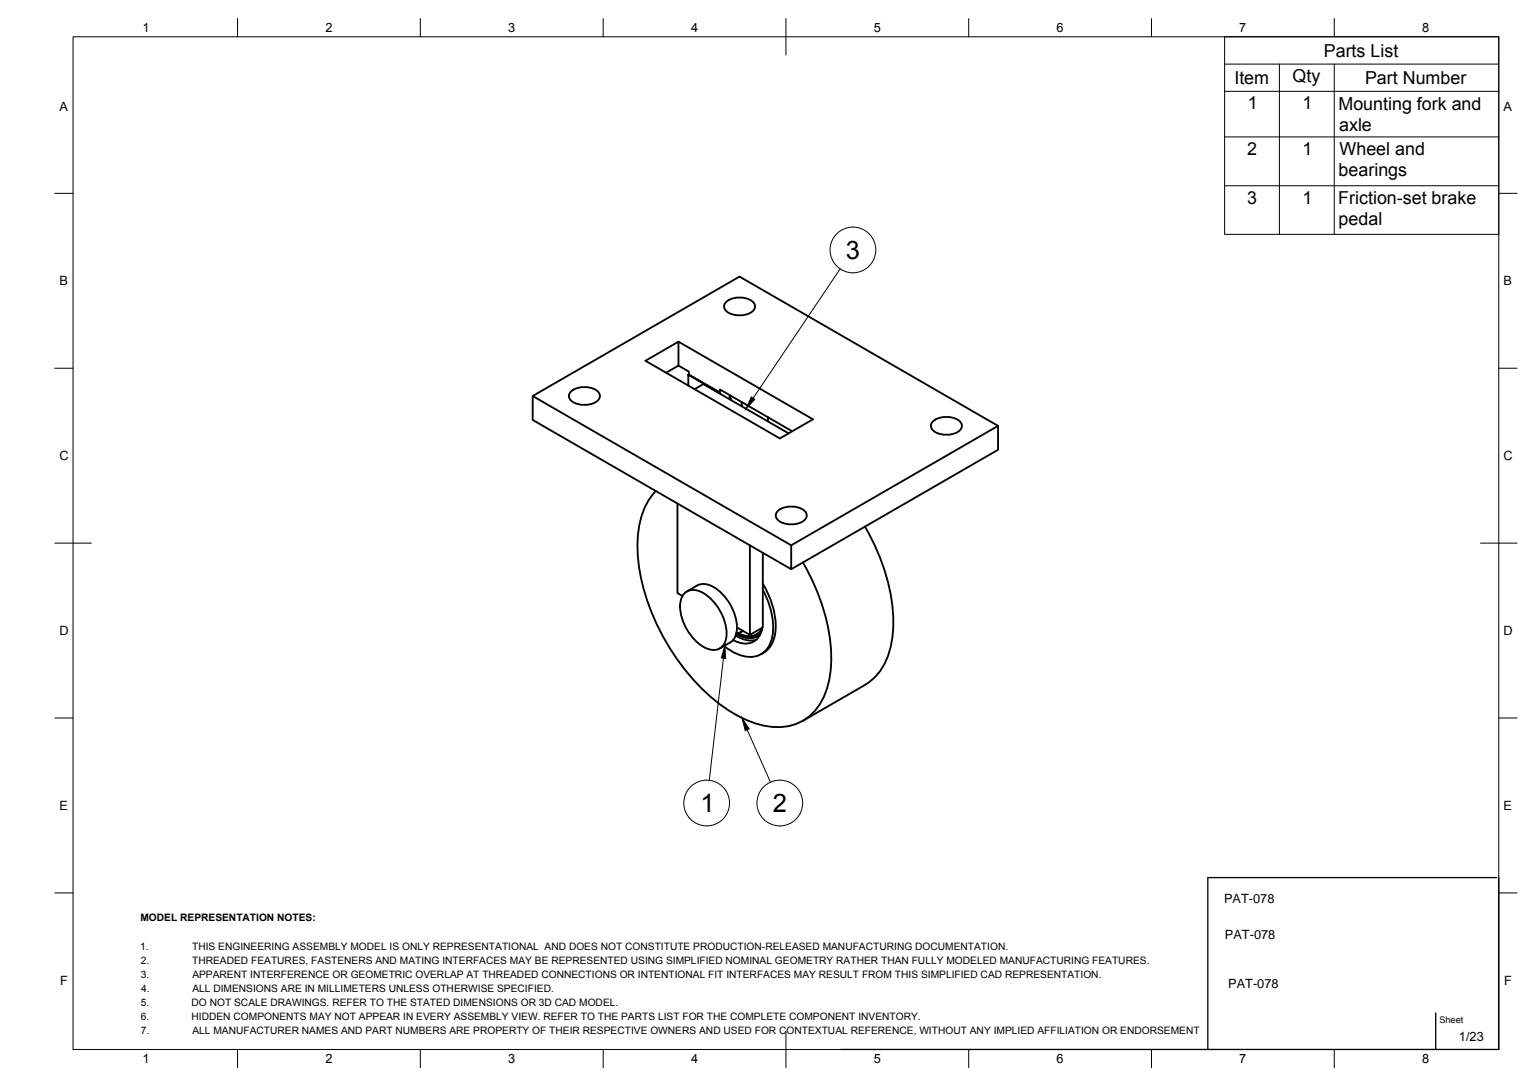
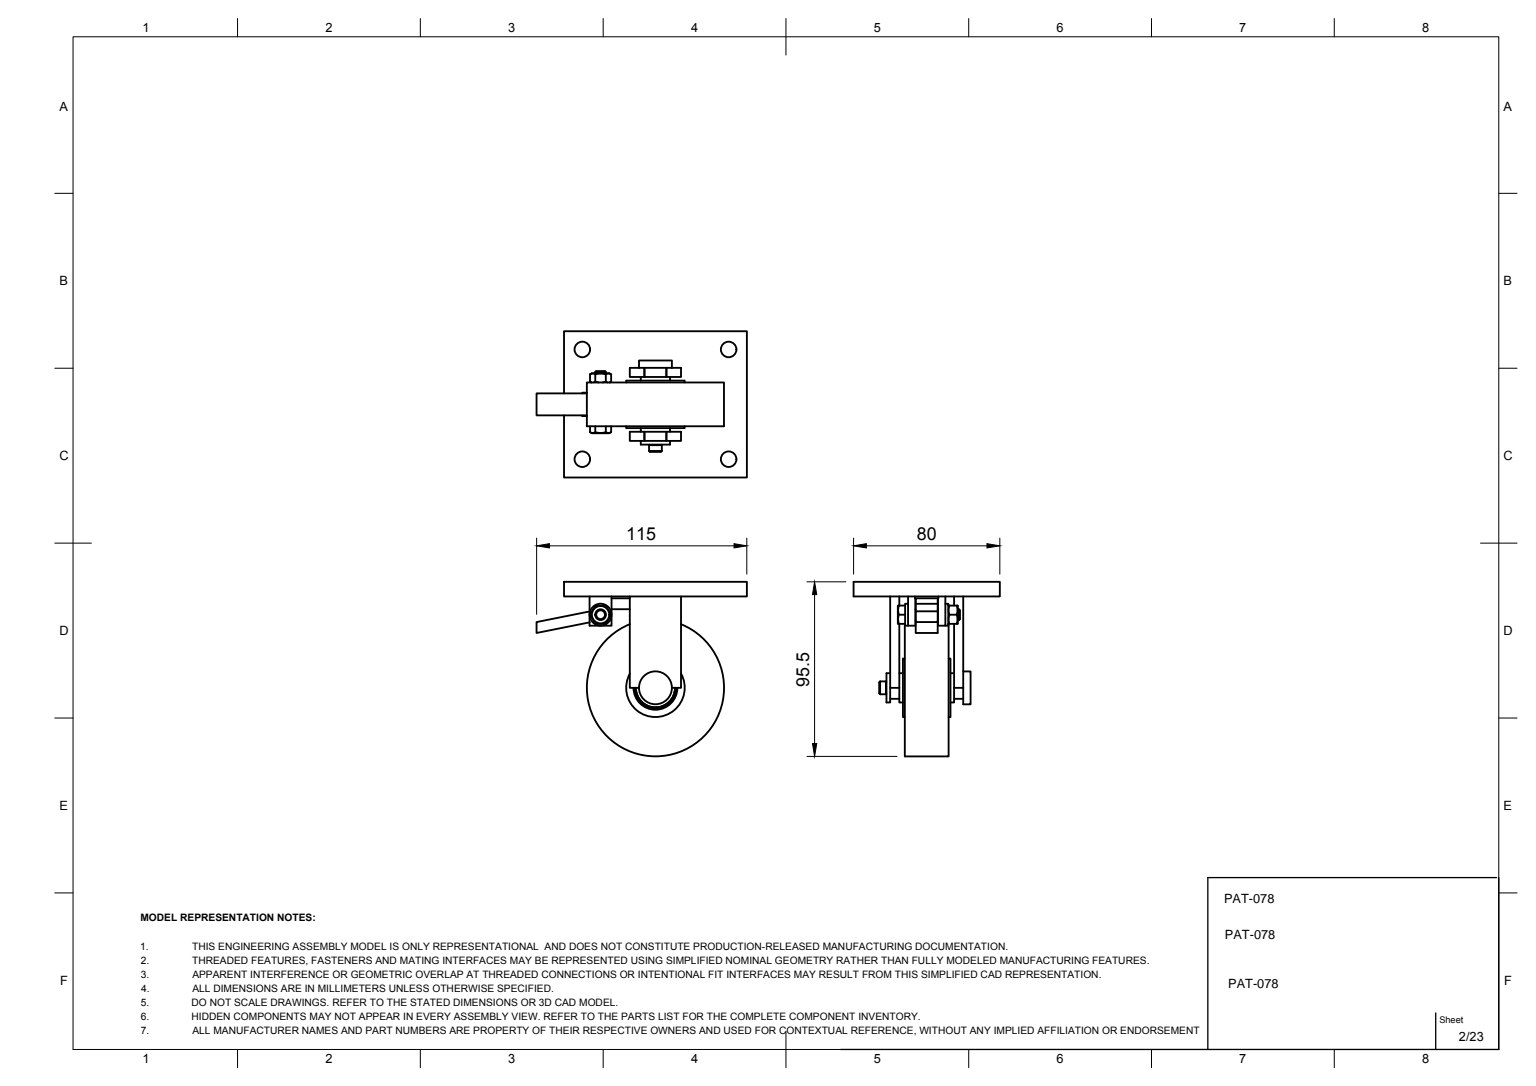
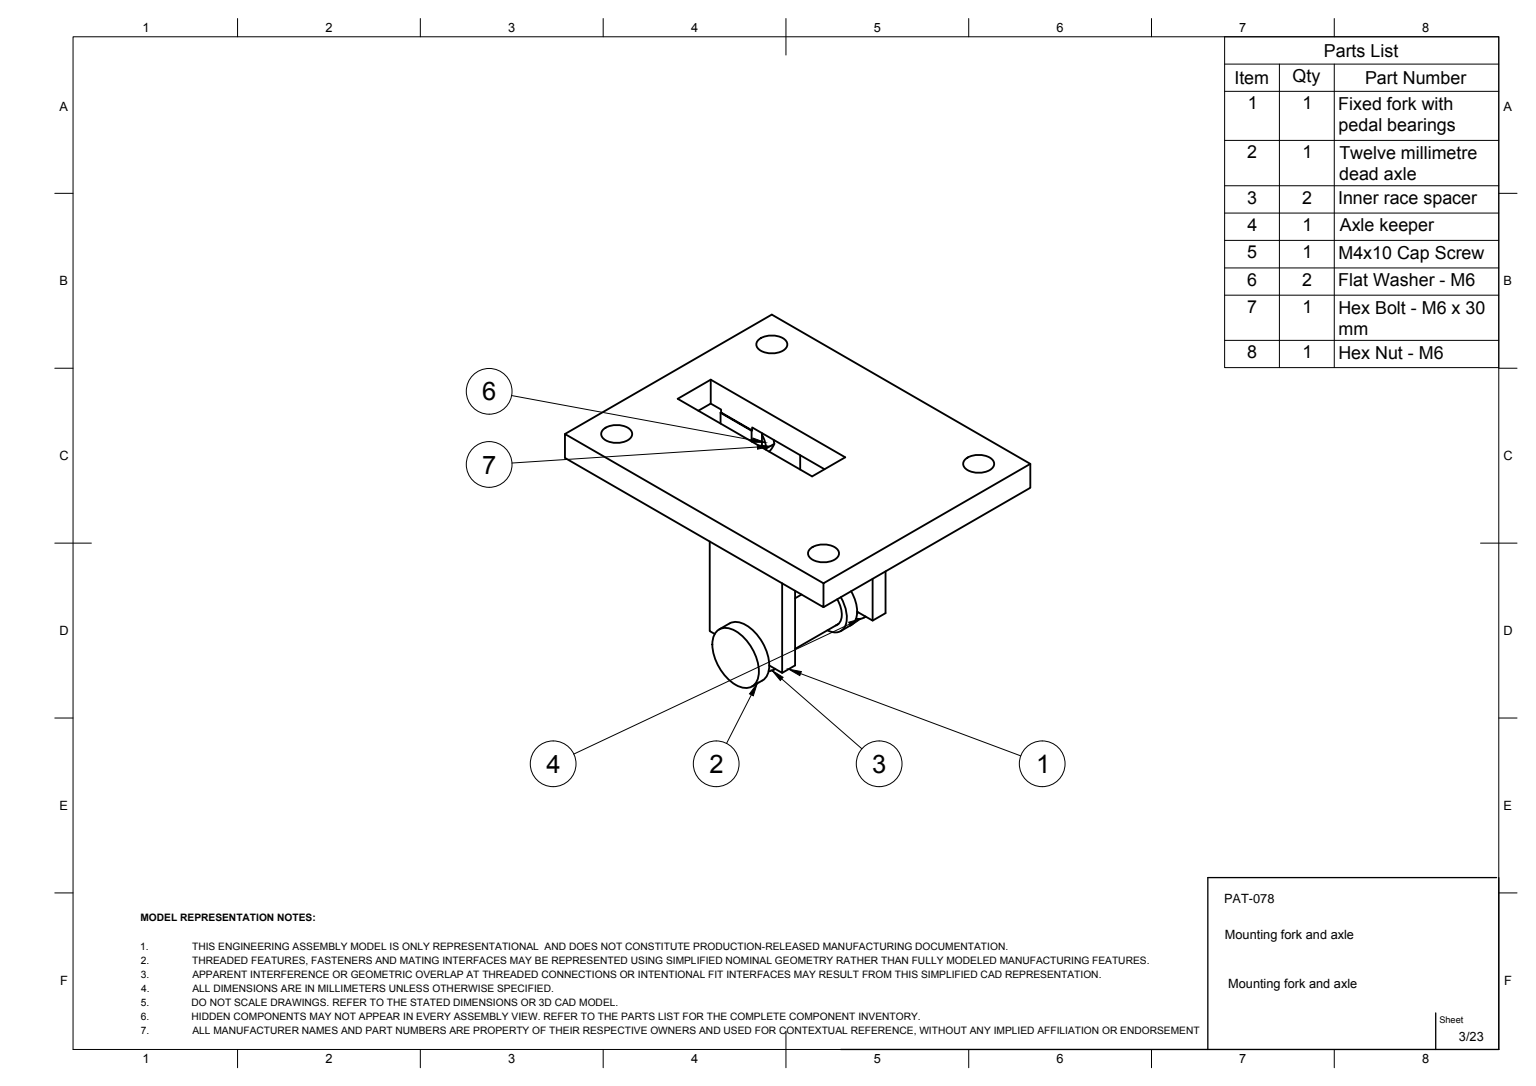
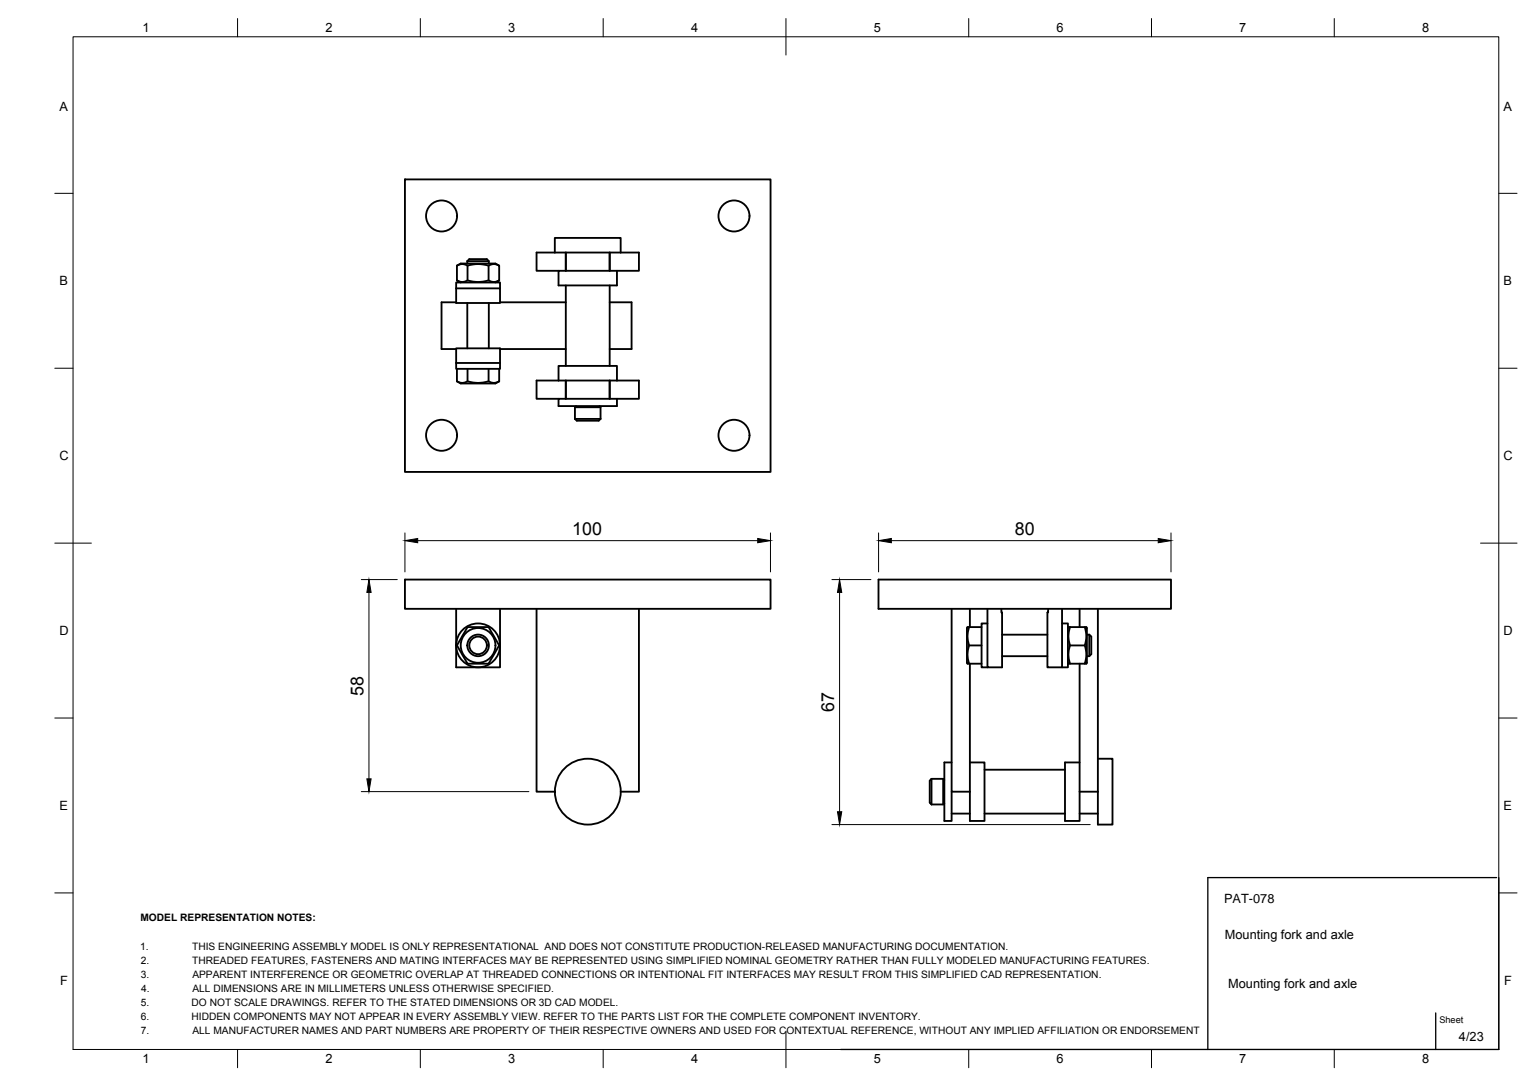
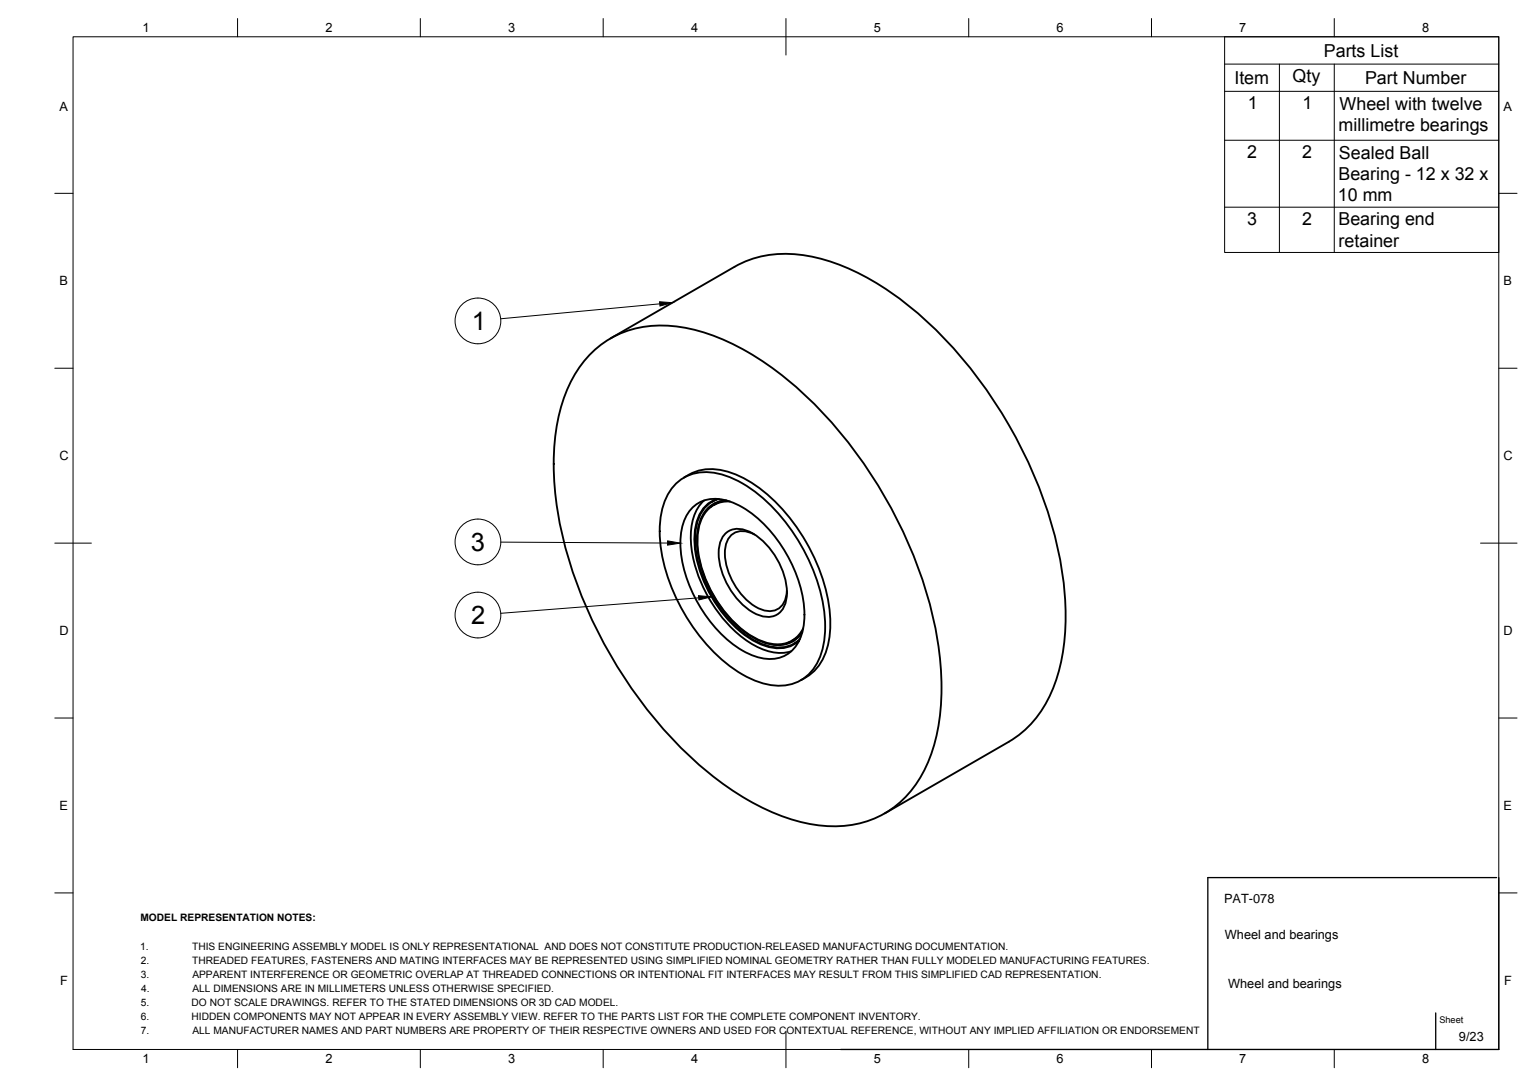
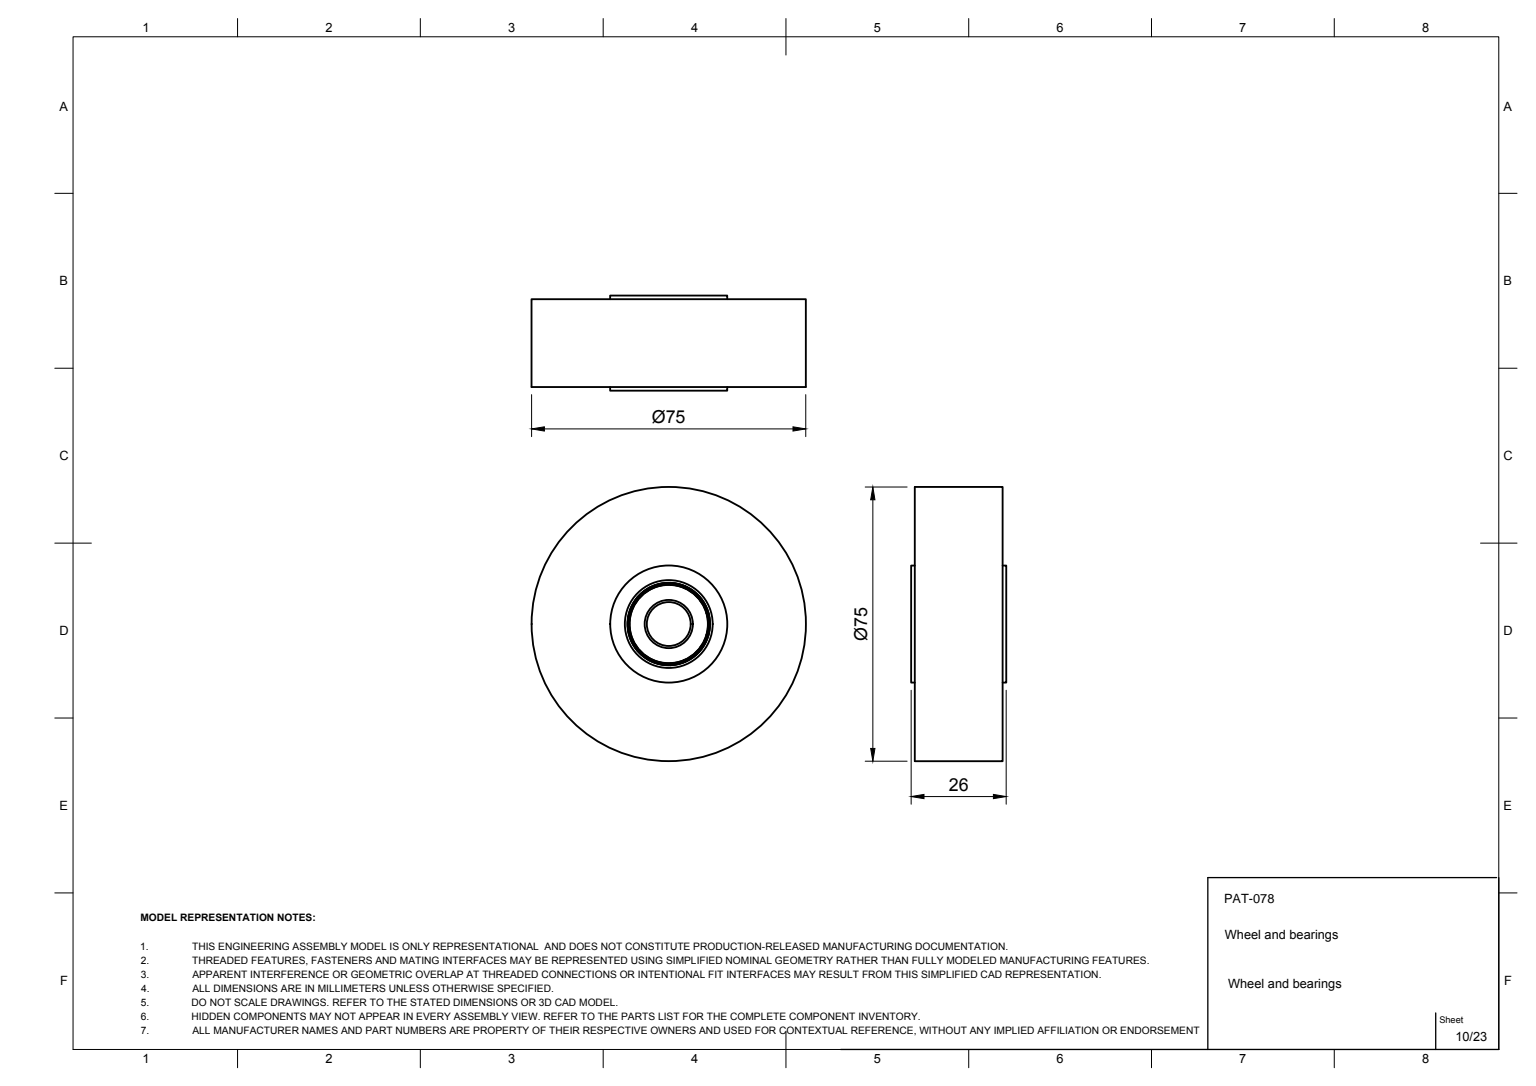
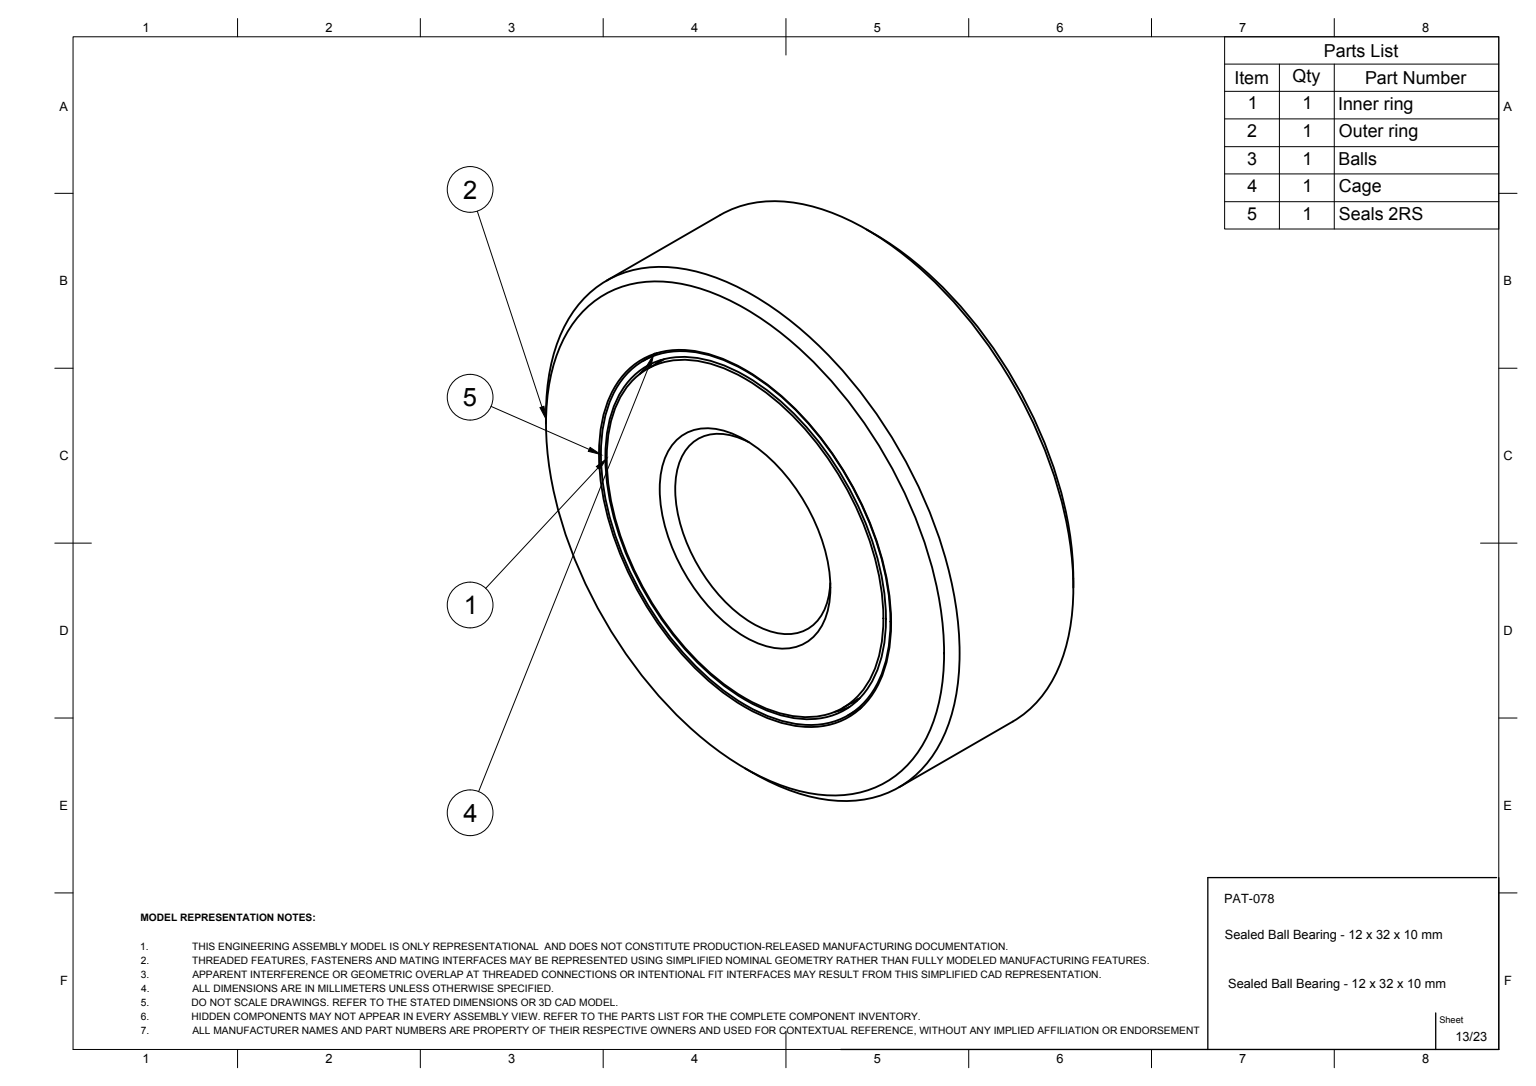
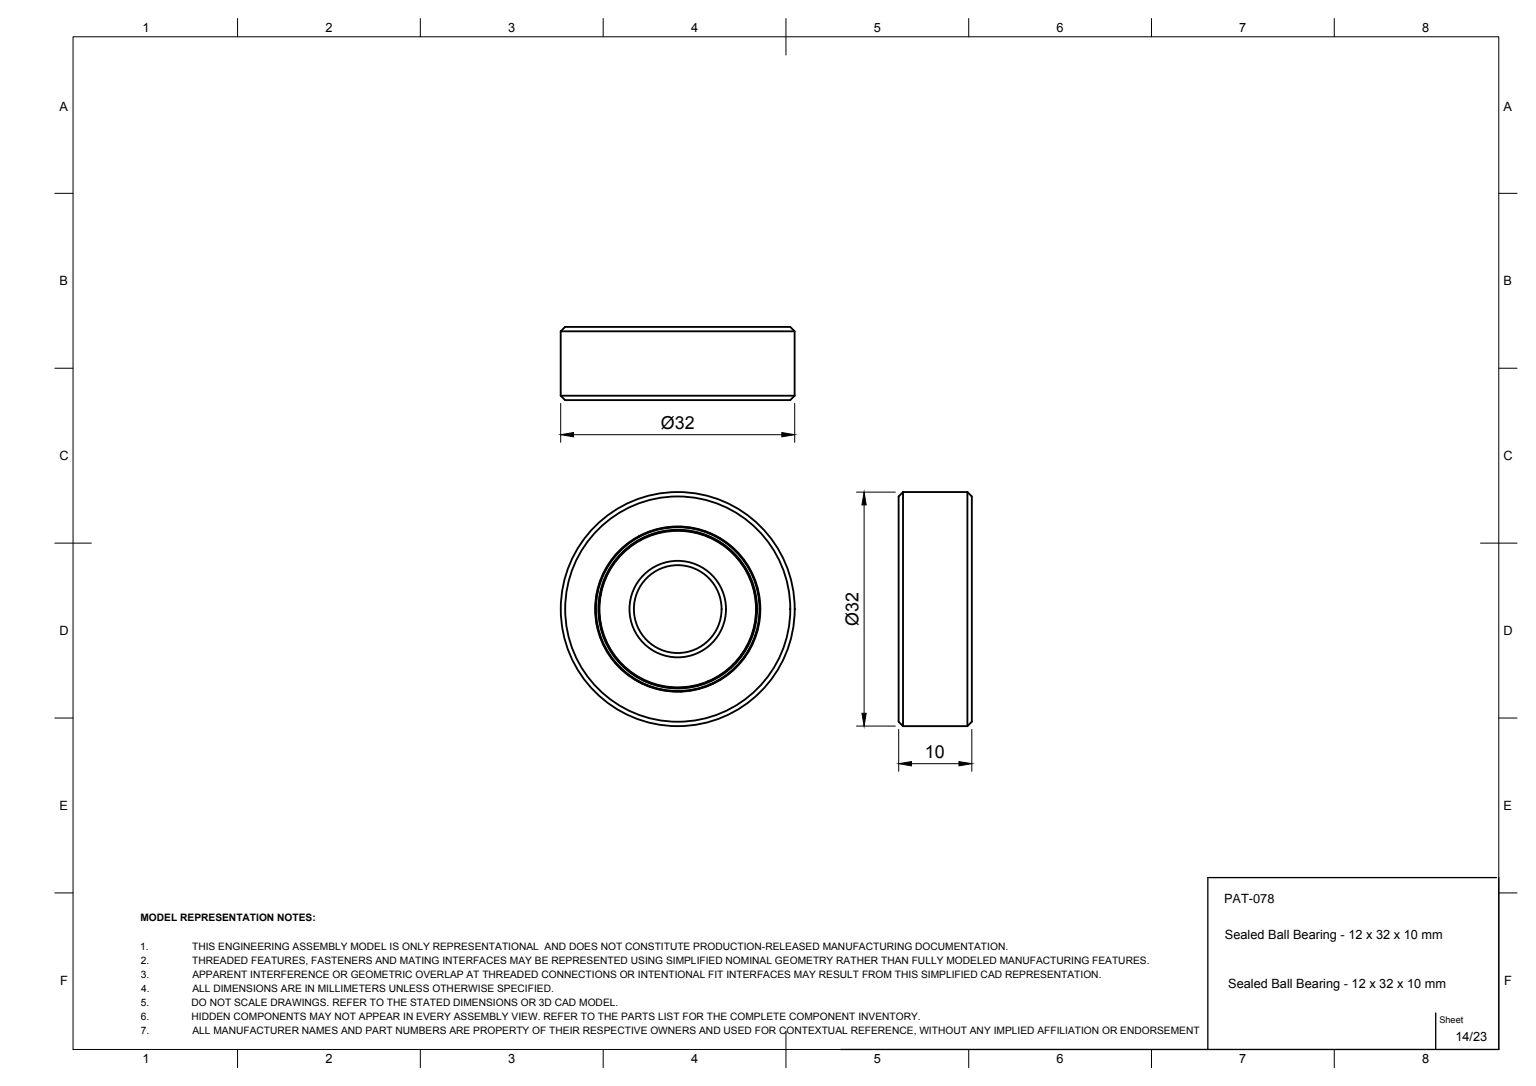
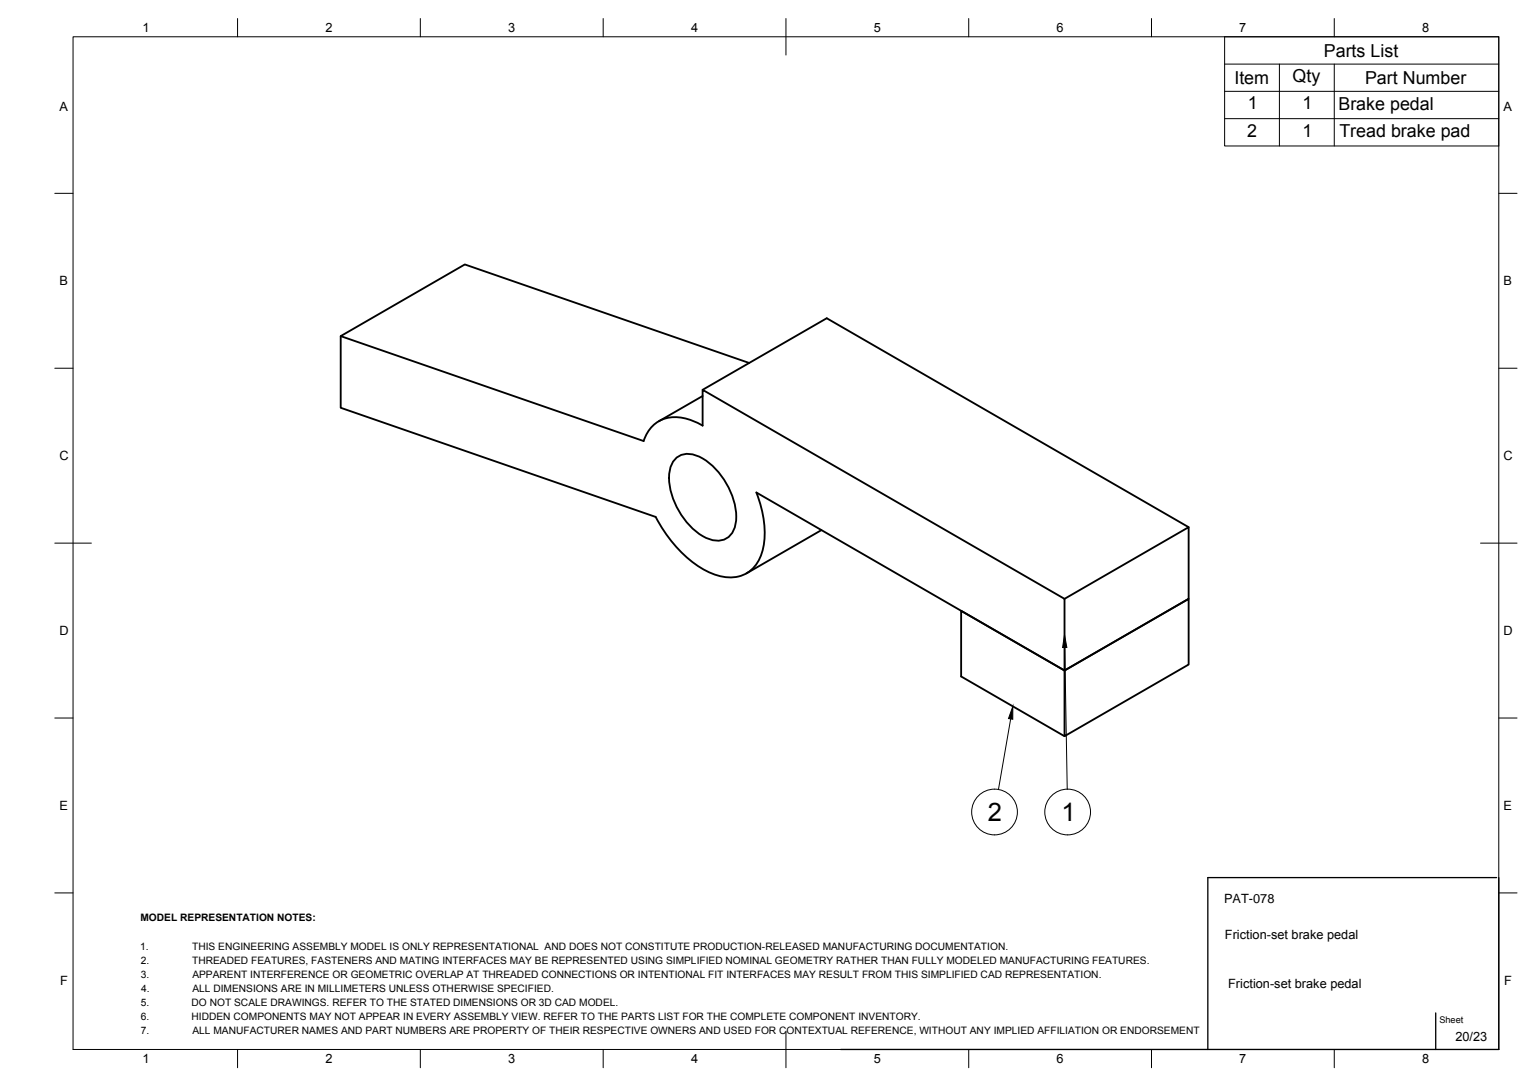
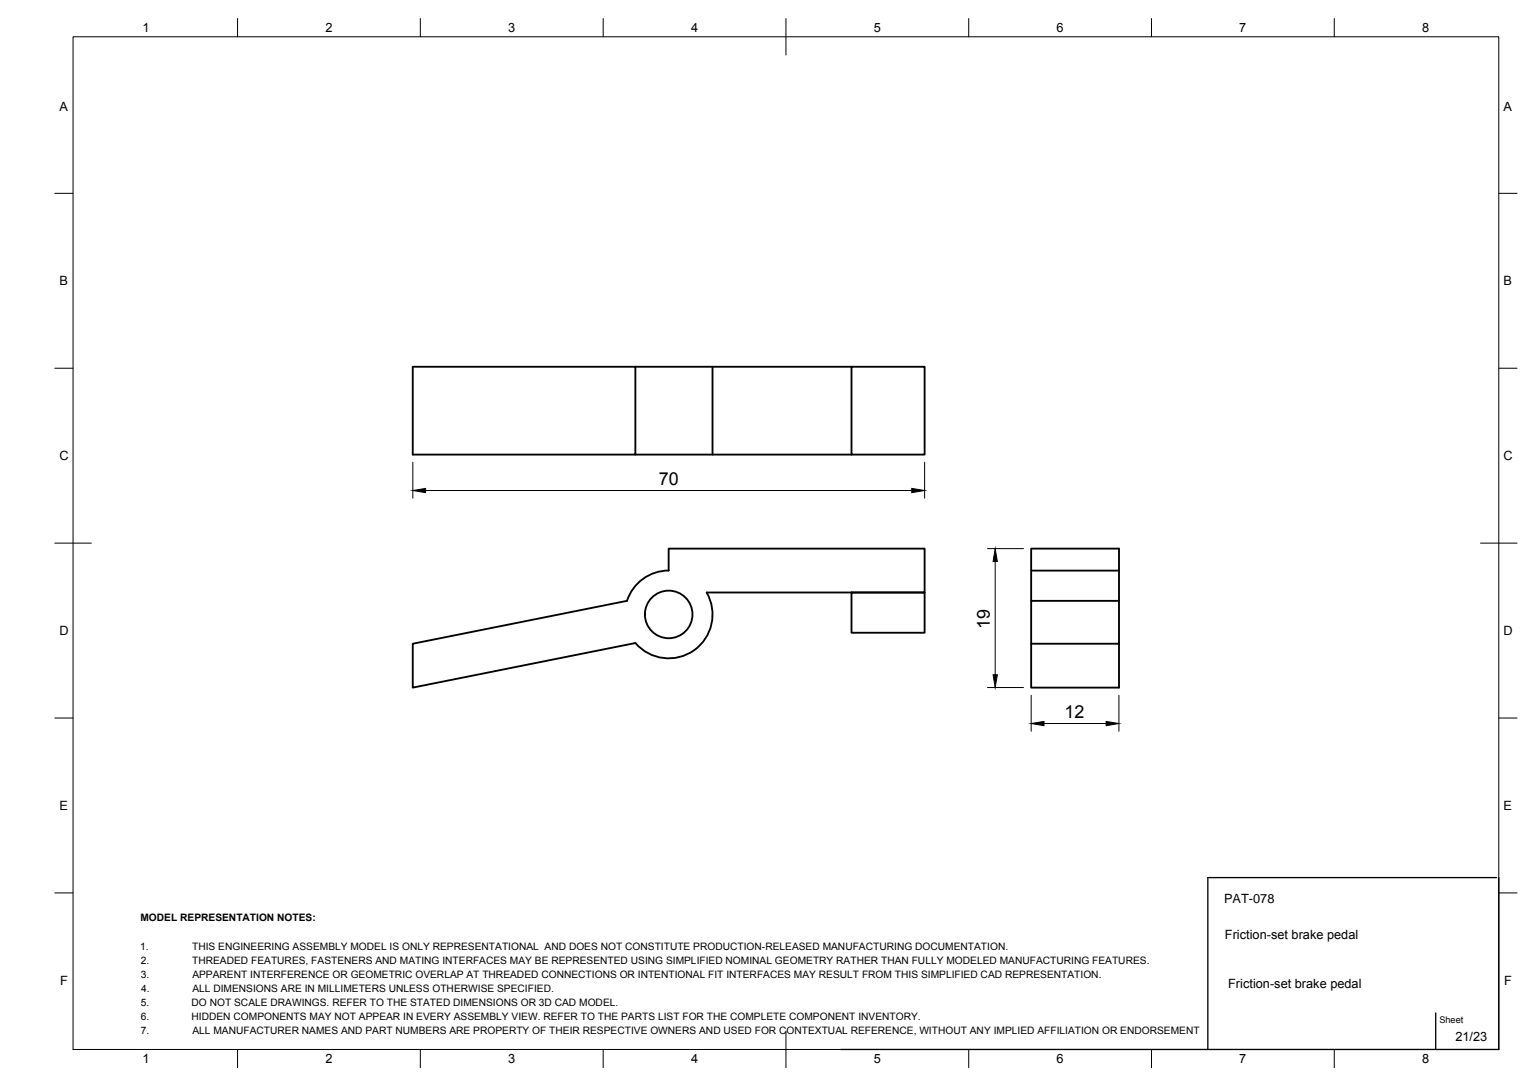
ISO-10303-21;
HEADER;
/* Generated by software containing ST-Developer
 * from STEP Tools, Inc. (www.steptools.com) 
 */

FILE_DESCRIPTION(
/* description */ ('Pedal-braked fixed caster'),
/* implementation_level */ '2;1');

FILE_NAME(
/* name */ 'PAT-078',
/* time_stamp */ '2026-10-28T03:26:52-07:00',
/* author */ (''),
/* organization */ (''),
/* preprocessor_version */ 'ST-DEVELOPER v20.2',
/* originating_system */ 'Autodesk Translation Framework v15.17.0.0',
/* authorisation */ '');

FILE_SCHEMA (('AUTOMOTIVE_DESIGN { 1 0 10303 214 3 1 1 }'));
ENDSEC;

DATA;
#10=MECHANICAL_DESIGN_GEOMETRIC_PRESENTATION_REPRESENTATION('',(#206,#207,
#208,#209,#210,#211,#212,#213,#214,#215,#216,#217,#218,#219,#220,#221,#222,
#223,#224,#225,#226,#227,#228,#229),#5734);
#11=B_SPLINE_CURVE_WITH_KNOTS('',3,(#5151,#5152,#5153,#5154,#5155,#5156,
#5157,#5158,#5159,#5160,#5161,#5162,#5163,#5164,#5165,#5166,#5167,#5168,
#5169,#5170,#5171,#5172),.UNSPECIFIED.,.F.,.F.,(4,2,2,2,2,2,2,2,2,2,4),
(0.0591825211272536,0.157966726598481,0.236950089897721,0.315933453196962,
0.391576304923761,0.46721915665056,0.54286200837736,0.618504860104159,0.697488223403399,
0.77647158670264,0.875255792173867),.UNSPECIFIED.);
#12=B_SPLINE_CURVE_WITH_KNOTS('',3,(#5176,#5177,#5178,#5179,#5180,#5181,
#5182,#5183,#5184,#5185,#5186,#5187,#5188,#5189,#5190,#5191,#5192,#5193,
#5194,#5195,#5196,#5197),.UNSPECIFIED.,.F.,.F.,(4,2,2,2,2,2,2,2,2,2,4),
(0.0581119756758434,0.106553146291161,0.213106292582322,0.30849933801665,
0.386091982889075,0.4636846277615,0.541277272633925,0.61886991750635,0.714262962940678,
0.820816109231839,0.869257279847157),.UNSPECIFIED.);
#13=B_SPLINE_CURVE_WITH_KNOTS('',3,(#5203,#5204,#5205,#5206,#5207,#5208,
#5209,#5210,#5211,#5212,#5213,#5214,#5215,#5216,#5217,#5218,#5219,#5220,
#5221,#5222,#5223,#5224),.UNSPECIFIED.,.F.,.F.,(4,2,2,2,2,2,2,2,2,2,4),
(0.0581119756758434,0.106553146291161,0.213106292582322,0.30849933801665,
0.386091982889075,0.4636846277615,0.541277272633925,0.61886991750635,0.714262962940679,
0.820816109231839,0.869257279847157),.UNSPECIFIED.);
#14=B_SPLINE_CURVE_WITH_KNOTS('',3,(#5228,#5229,#5230,#5231,#5232,#5233,
#5234,#5235,#5236,#5237,#5238,#5239,#5240,#5241,#5242,#5243,#5244,#5245,
#5246,#5247,#5248,#5249),.UNSPECIFIED.,.F.,.F.,(4,2,2,2,2,2,2,2,2,2,4),
(0.0581119756758433,0.106553146291161,0.213106292582322,0.308499338016649,
0.386091982889075,0.4636846277615,0.541277272633925,0.61886991750635,0.714262962940678,
0.820816109231839,0.869257279847157),.UNSPECIFIED.);
#15=B_SPLINE_CURVE_WITH_KNOTS('',3,(#5258,#5259,#5260,#5261,#5262,#5263,
#5264,#5265,#5266,#5267,#5268,#5269,#5270,#5271,#5272,#5273,#5274,#5275,
#5276,#5277,#5278,#5279),.UNSPECIFIED.,.F.,.F.,(4,2,2,2,2,2,2,2,2,2,4),
(0.0581119756758433,0.106553146291161,0.213106292582322,0.30849933801665,
0.386091982889075,0.4636846277615,0.541277272633925,0.61886991750635,0.714262962940678,
0.820816109231839,0.869257279847157),.UNSPECIFIED.);
#16=B_SPLINE_CURVE_WITH_KNOTS('',3,(#5283,#5284,#5285,#5286,#5287,#5288,
#5289,#5290,#5291,#5292,#5293,#5294,#5295,#5296,#5297,#5298,#5299,#5300,
#5301,#5302,#5303,#5304),.UNSPECIFIED.,.F.,.F.,(4,2,2,2,2,2,2,2,2,2,4),
(0.0581119756758434,0.106553146291161,0.213106292582322,0.30849933801665,
0.386091982889075,0.4636846277615,0.541277272633925,0.61886991750635,0.714262962940678,
0.820816109231839,0.869257279847157),.UNSPECIFIED.);
#17=B_SPLINE_CURVE_WITH_KNOTS('',3,(#5308,#5309,#5310,#5311,#5312,#5313,
#5314,#5315,#5316,#5317,#5318,#5319,#5320,#5321,#5322,#5323,#5324,#5325,
#5326,#5327,#5328,#5329),.UNSPECIFIED.,.F.,.F.,(4,2,2,2,2,2,2,2,2,2,4),
(0.0581119756758434,0.106553146291161,0.213106292582322,0.30849933801665,
0.386091982889075,0.4636846277615,0.541277272633925,0.61886991750635,0.714262962940678,
0.820816109231839,0.869257279847157),.UNSPECIFIED.);
#18=B_SPLINE_CURVE_WITH_KNOTS('',3,(#5333,#5334,#5335,#5336,#5337,#5338,
#5339,#5340,#5341,#5342,#5343,#5344,#5345,#5346,#5347,#5348,#5349,#5350,
#5351,#5352,#5353,#5354),.UNSPECIFIED.,.F.,.F.,(4,2,2,2,2,2,2,2,2,2,4),
(0.0581119756758433,0.106553146291161,0.213106292582322,0.30849933801665,
0.386091982889075,0.4636846277615,0.541277272633925,0.61886991750635,0.714262962940678,
0.820816109231839,0.869257279847157),.UNSPECIFIED.);
#19=B_SPLINE_CURVE_WITH_KNOTS('',3,(#5362,#5363,#5364,#5365,#5366,#5367,
#5368,#5369,#5370,#5371,#5372,#5373,#5374,#5375,#5376,#5377,#5378,#5379,
#5380,#5381,#5382,#5383),.UNSPECIFIED.,.F.,.F.,(4,2,2,2,2,2,2,2,2,2,4),
(0.0591825211272536,0.157966726598481,0.236950089897721,0.315933453196962,
0.391576304923761,0.467219156650561,0.54286200837736,0.618504860104159,
0.697488223403399,0.77647158670264,0.875255792173867),.UNSPECIFIED.);
#20=B_SPLINE_CURVE_WITH_KNOTS('',3,(#5391,#5392,#5393,#5394,#5395,#5396,
#5397,#5398,#5399,#5400,#5401,#5402,#5403,#5404,#5405,#5406,#5407,#5408,
#5409,#5410,#5411,#5412),.UNSPECIFIED.,.F.,.F.,(4,2,2,2,2,2,2,2,2,2,4),
(0.0591825211272536,0.157966726598481,0.236950089897722,0.315933453196962,
0.391576304923761,0.467219156650561,0.54286200837736,0.618504860104159,
0.697488223403399,0.77647158670264,0.875255792173867),.UNSPECIFIED.);
#21=B_SPLINE_CURVE_WITH_KNOTS('',3,(#5422,#5423,#5424,#5425,#5426,#5427,
#5428,#5429,#5430,#5431,#5432,#5433,#5434,#5435,#5436,#5437,#5438,#5439,
#5440,#5441,#5442,#5443),.UNSPECIFIED.,.F.,.F.,(4,2,2,2,2,2,2,2,2,2,4),
(0.0591825211272536,0.157966726598481,0.236950089897721,0.315933453196962,
0.391576304923761,0.46721915665056,0.54286200837736,0.618504860104159,0.697488223403399,
0.77647158670264,0.875255792173867),.UNSPECIFIED.);
#22=B_SPLINE_CURVE_WITH_KNOTS('',3,(#5451,#5452,#5453,#5454,#5455,#5456,
#5457,#5458,#5459,#5460,#5461,#5462,#5463,#5464,#5465,#5466,#5467,#5468,
#5469,#5470,#5471,#5472),.UNSPECIFIED.,.F.,.F.,(4,2,2,2,2,2,2,2,2,2,4),
(0.0591825211272536,0.157966726598481,0.236950089897721,0.315933453196962,
0.391576304923761,0.46721915665056,0.542862008377359,0.618504860104159,
0.697488223403399,0.776471586702639,0.875255792173867),.UNSPECIFIED.);
#23=B_SPLINE_CURVE_WITH_KNOTS('',3,(#5480,#5481,#5482,#5483,#5484,#5485,
#5486,#5487,#5488,#5489,#5490,#5491,#5492,#5493,#5494,#5495,#5496,#5497,
#5498,#5499,#5500,#5501),.UNSPECIFIED.,.F.,.F.,(4,2,2,2,2,2,2,2,2,2,4),
(0.0591825211272536,0.157966726598481,0.236950089897721,0.315933453196962,
0.391576304923761,0.46721915665056,0.54286200837736,0.618504860104159,0.697488223403399,
0.77647158670264,0.875255792173867),.UNSPECIFIED.);
#24=B_SPLINE_CURVE_WITH_KNOTS('',3,(#5510,#5511,#5512,#5513,#5514,#5515,
#5516,#5517,#5518,#5519,#5520,#5521,#5522,#5523,#5524,#5525,#5526,#5527,
#5528,#5529,#5530,#5531),.UNSPECIFIED.,.F.,.F.,(4,2,2,2,2,2,2,2,2,2,4),
(0.0591825211272536,0.157966726598481,0.236950089897721,0.315933453196962,
0.391576304923761,0.46721915665056,0.542862008377359,0.618504860104159,
0.697488223403399,0.776471586702639,0.875255792173867),.UNSPECIFIED.);
#25=SPHERICAL_SURFACE('',#3429,0.29765);
#26=SPHERICAL_SURFACE('',#3431,0.29765);
#27=SPHERICAL_SURFACE('',#3433,0.29765);
#28=SPHERICAL_SURFACE('',#3435,0.29765);
#29=SPHERICAL_SURFACE('',#3437,0.29765);
#30=SPHERICAL_SURFACE('',#3439,0.29765);
#31=SPHERICAL_SURFACE('',#3441,0.29765);
#32=SPHERICAL_SURFACE('',#3444,0.309556);
#33=SPHERICAL_SURFACE('',#3460,0.309556);
#34=SPHERICAL_SURFACE('',#3465,0.309556);
#35=SPHERICAL_SURFACE('',#3471,0.309556);
#36=SPHERICAL_SURFACE('',#3476,0.309556);
#37=SPHERICAL_SURFACE('',#3481,0.309556);
#38=SPHERICAL_SURFACE('',#3489,0.309556);
#39=TOROIDAL_SURFACE('',#3389,1.1,0.309556);
#40=TOROIDAL_SURFACE('',#3409,1.1,0.309556);
#41=ITEM_DEFINED_TRANSFORMATION($,$,#3202,#3359);
#42=ITEM_DEFINED_TRANSFORMATION($,$,#3261,#3360);
#43=ITEM_DEFINED_TRANSFORMATION($,$,#3275,#3361);
#44=ITEM_DEFINED_TRANSFORMATION($,$,#3275,#3362);
#45=ITEM_DEFINED_TRANSFORMATION($,$,#3284,#3363);
#46=ITEM_DEFINED_TRANSFORMATION($,$,#3293,#3364);
#47=ITEM_DEFINED_TRANSFORMATION($,$,#3317,#3365);
#48=ITEM_DEFINED_TRANSFORMATION($,$,#3317,#3366);
#49=ITEM_DEFINED_TRANSFORMATION($,$,#3326,#3367);
#50=ITEM_DEFINED_TRANSFORMATION($,$,#3343,#3368);
#51=ITEM_DEFINED_TRANSFORMATION($,$,#3388,#3510);
#52=ITEM_DEFINED_TRANSFORMATION($,$,#3408,#3511);
#53=ITEM_DEFINED_TRANSFORMATION($,$,#3428,#3512);
#54=ITEM_DEFINED_TRANSFORMATION($,$,#3443,#3513);
#55=ITEM_DEFINED_TRANSFORMATION($,$,#3493,#3514);
#56=ITEM_DEFINED_TRANSFORMATION($,$,#3370,#3524);
#57=ITEM_DEFINED_TRANSFORMATION($,$,#3387,#3525);
#58=ITEM_DEFINED_TRANSFORMATION($,$,#3387,#3526);
#59=ITEM_DEFINED_TRANSFORMATION($,$,#3515,#3527);
#60=ITEM_DEFINED_TRANSFORMATION($,$,#3515,#3528);
#61=ITEM_DEFINED_TRANSFORMATION($,$,#3530,#3556);
#62=ITEM_DEFINED_TRANSFORMATION($,$,#3549,#3557);
#63=ITEM_DEFINED_TRANSFORMATION($,$,#3201,#3558);
#64=ITEM_DEFINED_TRANSFORMATION($,$,#3369,#3559);
#65=ITEM_DEFINED_TRANSFORMATION($,$,#3529,#3560);
#66=(
REPRESENTATION_RELATIONSHIP($,$,#5810,#5809)
REPRESENTATION_RELATIONSHIP_WITH_TRANSFORMATION(#41)
SHAPE_REPRESENTATION_RELATIONSHIP()
);
#67=(
REPRESENTATION_RELATIONSHIP($,$,#5811,#5809)
REPRESENTATION_RELATIONSHIP_WITH_TRANSFORMATION(#42)
SHAPE_REPRESENTATION_RELATIONSHIP()
);
#68=(
REPRESENTATION_RELATIONSHIP($,$,#5812,#5809)
REPRESENTATION_RELATIONSHIP_WITH_TRANSFORMATION(#43)
SHAPE_REPRESENTATION_RELATIONSHIP()
);
#69=(
REPRESENTATION_RELATIONSHIP($,$,#5812,#5809)
REPRESENTATION_RELATIONSHIP_WITH_TRANSFORMATION(#44)
SHAPE_REPRESENTATION_RELATIONSHIP()
);
#70=(
REPRESENTATION_RELATIONSHIP($,$,#5813,#5809)
REPRESENTATION_RELATIONSHIP_WITH_TRANSFORMATION(#45)
SHAPE_REPRESENTATION_RELATIONSHIP()
);
#71=(
REPRESENTATION_RELATIONSHIP($,$,#5814,#5809)
REPRESENTATION_RELATIONSHIP_WITH_TRANSFORMATION(#46)
SHAPE_REPRESENTATION_RELATIONSHIP()
);
#72=(
REPRESENTATION_RELATIONSHIP($,$,#5815,#5809)
REPRESENTATION_RELATIONSHIP_WITH_TRANSFORMATION(#47)
SHAPE_REPRESENTATION_RELATIONSHIP()
);
#73=(
REPRESENTATION_RELATIONSHIP($,$,#5815,#5809)
REPRESENTATION_RELATIONSHIP_WITH_TRANSFORMATION(#48)
SHAPE_REPRESENTATION_RELATIONSHIP()
);
#74=(
REPRESENTATION_RELATIONSHIP($,$,#5816,#5809)
REPRESENTATION_RELATIONSHIP_WITH_TRANSFORMATION(#49)
SHAPE_REPRESENTATION_RELATIONSHIP()
);
#75=(
REPRESENTATION_RELATIONSHIP($,$,#5817,#5809)
REPRESENTATION_RELATIONSHIP_WITH_TRANSFORMATION(#50)
SHAPE_REPRESENTATION_RELATIONSHIP()
);
#76=(
REPRESENTATION_RELATIONSHIP($,$,#5821,#5820)
REPRESENTATION_RELATIONSHIP_WITH_TRANSFORMATION(#51)
SHAPE_REPRESENTATION_RELATIONSHIP()
);
#77=(
REPRESENTATION_RELATIONSHIP($,$,#5822,#5820)
REPRESENTATION_RELATIONSHIP_WITH_TRANSFORMATION(#52)
SHAPE_REPRESENTATION_RELATIONSHIP()
);
#78=(
REPRESENTATION_RELATIONSHIP($,$,#5823,#5820)
REPRESENTATION_RELATIONSHIP_WITH_TRANSFORMATION(#53)
SHAPE_REPRESENTATION_RELATIONSHIP()
);
#79=(
REPRESENTATION_RELATIONSHIP($,$,#5824,#5820)
REPRESENTATION_RELATIONSHIP_WITH_TRANSFORMATION(#54)
SHAPE_REPRESENTATION_RELATIONSHIP()
);
#80=(
REPRESENTATION_RELATIONSHIP($,$,#5825,#5820)
REPRESENTATION_RELATIONSHIP_WITH_TRANSFORMATION(#55)
SHAPE_REPRESENTATION_RELATIONSHIP()
);
#81=(
REPRESENTATION_RELATIONSHIP($,$,#5819,#5818)
REPRESENTATION_RELATIONSHIP_WITH_TRANSFORMATION(#56)
SHAPE_REPRESENTATION_RELATIONSHIP()
);
#82=(
REPRESENTATION_RELATIONSHIP($,$,#5820,#5818)
REPRESENTATION_RELATIONSHIP_WITH_TRANSFORMATION(#57)
SHAPE_REPRESENTATION_RELATIONSHIP()
);
#83=(
REPRESENTATION_RELATIONSHIP($,$,#5820,#5818)
REPRESENTATION_RELATIONSHIP_WITH_TRANSFORMATION(#58)
SHAPE_REPRESENTATION_RELATIONSHIP()
);
#84=(
REPRESENTATION_RELATIONSHIP($,$,#5826,#5818)
REPRESENTATION_RELATIONSHIP_WITH_TRANSFORMATION(#59)
SHAPE_REPRESENTATION_RELATIONSHIP()
);
#85=(
REPRESENTATION_RELATIONSHIP($,$,#5826,#5818)
REPRESENTATION_RELATIONSHIP_WITH_TRANSFORMATION(#60)
SHAPE_REPRESENTATION_RELATIONSHIP()
);
#86=(
REPRESENTATION_RELATIONSHIP($,$,#5828,#5827)
REPRESENTATION_RELATIONSHIP_WITH_TRANSFORMATION(#61)
SHAPE_REPRESENTATION_RELATIONSHIP()
);
#87=(
REPRESENTATION_RELATIONSHIP($,$,#5829,#5827)
REPRESENTATION_RELATIONSHIP_WITH_TRANSFORMATION(#62)
SHAPE_REPRESENTATION_RELATIONSHIP()
);
#88=(
REPRESENTATION_RELATIONSHIP($,$,#5809,#5808)
REPRESENTATION_RELATIONSHIP_WITH_TRANSFORMATION(#63)
SHAPE_REPRESENTATION_RELATIONSHIP()
);
#89=(
REPRESENTATION_RELATIONSHIP($,$,#5818,#5808)
REPRESENTATION_RELATIONSHIP_WITH_TRANSFORMATION(#64)
SHAPE_REPRESENTATION_RELATIONSHIP()
);
#90=(
REPRESENTATION_RELATIONSHIP($,$,#5827,#5808)
REPRESENTATION_RELATIONSHIP_WITH_TRANSFORMATION(#65)
SHAPE_REPRESENTATION_RELATIONSHIP()
);
#91=CONTEXT_DEPENDENT_SHAPE_REPRESENTATION(#66,#5771);
#92=CONTEXT_DEPENDENT_SHAPE_REPRESENTATION(#67,#5772);
#93=CONTEXT_DEPENDENT_SHAPE_REPRESENTATION(#68,#5773);
#94=CONTEXT_DEPENDENT_SHAPE_REPRESENTATION(#69,#5774);
#95=CONTEXT_DEPENDENT_SHAPE_REPRESENTATION(#70,#5775);
#96=CONTEXT_DEPENDENT_SHAPE_REPRESENTATION(#71,#5776);
#97=CONTEXT_DEPENDENT_SHAPE_REPRESENTATION(#72,#5777);
#98=CONTEXT_DEPENDENT_SHAPE_REPRESENTATION(#73,#5778);
#99=CONTEXT_DEPENDENT_SHAPE_REPRESENTATION(#74,#5779);
#100=CONTEXT_DEPENDENT_SHAPE_REPRESENTATION(#75,#5780);
#101=CONTEXT_DEPENDENT_SHAPE_REPRESENTATION(#76,#5789);
#102=CONTEXT_DEPENDENT_SHAPE_REPRESENTATION(#77,#5790);
#103=CONTEXT_DEPENDENT_SHAPE_REPRESENTATION(#78,#5791);
#104=CONTEXT_DEPENDENT_SHAPE_REPRESENTATION(#79,#5792);
#105=CONTEXT_DEPENDENT_SHAPE_REPRESENTATION(#80,#5793);
#106=CONTEXT_DEPENDENT_SHAPE_REPRESENTATION(#81,#5795);
#107=CONTEXT_DEPENDENT_SHAPE_REPRESENTATION(#82,#5796);
#108=CONTEXT_DEPENDENT_SHAPE_REPRESENTATION(#83,#5797);
#109=CONTEXT_DEPENDENT_SHAPE_REPRESENTATION(#84,#5798);
#110=CONTEXT_DEPENDENT_SHAPE_REPRESENTATION(#85,#5799);
#111=CONTEXT_DEPENDENT_SHAPE_REPRESENTATION(#86,#5803);
#112=CONTEXT_DEPENDENT_SHAPE_REPRESENTATION(#87,#5804);
#113=CONTEXT_DEPENDENT_SHAPE_REPRESENTATION(#88,#5805);
#114=CONTEXT_DEPENDENT_SHAPE_REPRESENTATION(#89,#5806);
#115=CONTEXT_DEPENDENT_SHAPE_REPRESENTATION(#90,#5807);
#116=NEXT_ASSEMBLY_USAGE_OCCURRENCE('Fixed fork with pedal bearings:1',
'Fixed fork with pedal bearings:1','Fixed fork with pedal bearings:1',#5832,
#5833,'Fixed fork with pedal bearings:1');
#117=NEXT_ASSEMBLY_USAGE_OCCURRENCE('Twelve millimetre dead axle:2',
'Twelve millimetre dead axle:2','Twelve millimetre dead axle:2',#5832,#5834,
'Twelve millimetre dead axle:2');
#118=NEXT_ASSEMBLY_USAGE_OCCURRENCE('Inner race spacer:2',
'Inner race spacer:2','Inner race spacer:2',#5832,#5835,
'Inner race spacer:2');
#119=NEXT_ASSEMBLY_USAGE_OCCURRENCE('Inner race spacer:3',
'Inner race spacer:3','Inner race spacer:3',#5832,#5835,
'Inner race spacer:3');
#120=NEXT_ASSEMBLY_USAGE_OCCURRENCE('Axle keeper:2','Axle keeper:2',
'Axle keeper:2',#5832,#5836,'Axle keeper:2');
#121=NEXT_ASSEMBLY_USAGE_OCCURRENCE('M4x10 Cap Screw:2',
'M4x10 Cap Screw:2','M4x10 Cap Screw:2',#5832,#5837,'M4x10 Cap Screw:2');
#122=NEXT_ASSEMBLY_USAGE_OCCURRENCE('Flat Washer - M6:2',
'Flat Washer - M6:2','Flat Washer - M6:2',#5832,#5838,
'Flat Washer - M6:2');
#123=NEXT_ASSEMBLY_USAGE_OCCURRENCE('Flat Washer - M6:3',
'Flat Washer - M6:3','Flat Washer - M6:3',#5832,#5838,
'Flat Washer - M6:3');
#124=NEXT_ASSEMBLY_USAGE_OCCURRENCE('Hex Bolt - M6 x 30 mm:2',
'Hex Bolt - M6 x 30 mm:2','Hex Bolt - M6 x 30 mm:2',#5832,#5839,
'Hex Bolt - M6 x 30 mm:2');
#125=NEXT_ASSEMBLY_USAGE_OCCURRENCE('Hex Nut - M6:2','Hex Nut - M6:2',
'Hex Nut - M6:2',#5832,#5840,'Hex Nut - M6:2');
#126=NEXT_ASSEMBLY_USAGE_OCCURRENCE('Inner ring:1','Inner ring:1',
'Inner ring:1',#5843,#5844,'Inner ring:1');
#127=NEXT_ASSEMBLY_USAGE_OCCURRENCE('Outer ring:1','Outer ring:1',
'Outer ring:1',#5843,#5845,'Outer ring:1');
#128=NEXT_ASSEMBLY_USAGE_OCCURRENCE('Balls:1','Balls:1','Balls:1',#5843,
#5846,'Balls:1');
#129=NEXT_ASSEMBLY_USAGE_OCCURRENCE('Cage:1','Cage:1','Cage:1',#5843,#5847,
'Cage:1');
#130=NEXT_ASSEMBLY_USAGE_OCCURRENCE('Seals 2RS:1','Seals 2RS:1',
'Seals 2RS:1',#5843,#5848,'Seals 2RS:1');
#131=NEXT_ASSEMBLY_USAGE_OCCURRENCE(
'Wheel with twelve millimetre bearings:2',
'Wheel with twelve millimetre bearings:2',
'Wheel with twelve millimetre bearings:2',#5841,#5842,
'Wheel with twelve millimetre bearings:2');
#132=NEXT_ASSEMBLY_USAGE_OCCURRENCE(
'Sealed Ball Bearing - 12 x 32 x 10 mm:2',
'Sealed Ball Bearing - 12 x 32 x 10 mm:2',
'Sealed Ball Bearing - 12 x 32 x 10 mm:2',#5841,#5843,
'Sealed Ball Bearing - 12 x 32 x 10 mm:2');
#133=NEXT_ASSEMBLY_USAGE_OCCURRENCE(
'Sealed Ball Bearing - 12 x 32 x 10 mm:3',
'Sealed Ball Bearing - 12 x 32 x 10 mm:3',
'Sealed Ball Bearing - 12 x 32 x 10 mm:3',#5841,#5843,
'Sealed Ball Bearing - 12 x 32 x 10 mm:3');
#134=NEXT_ASSEMBLY_USAGE_OCCURRENCE('Bearing end retainer:2',
'Bearing end retainer:2','Bearing end retainer:2',#5841,#5849,
'Bearing end retainer:2');
#135=NEXT_ASSEMBLY_USAGE_OCCURRENCE('Bearing end retainer:3',
'Bearing end retainer:3','Bearing end retainer:3',#5841,#5849,
'Bearing end retainer:3');
#136=NEXT_ASSEMBLY_USAGE_OCCURRENCE('Brake pedal:1','Brake pedal:1',
'Brake pedal:1',#5850,#5851,'Brake pedal:1');
#137=NEXT_ASSEMBLY_USAGE_OCCURRENCE('Tread brake pad:1',
'Tread brake pad:1','Tread brake pad:1',#5850,#5852,'Tread brake pad:1');
#138=NEXT_ASSEMBLY_USAGE_OCCURRENCE('Mounting fork and axle:1',
'Mounting fork and axle:1','Mounting fork and axle:1',#5831,#5832,
'Mounting fork and axle:1');
#139=NEXT_ASSEMBLY_USAGE_OCCURRENCE('Wheel and bearings:1',
'Wheel and bearings:1','Wheel and bearings:1',#5831,#5841,
'Wheel and bearings:1');
#140=NEXT_ASSEMBLY_USAGE_OCCURRENCE('Friction-set brake pedal:1',
'Friction-set brake pedal:1','Friction-set brake pedal:1',#5831,#5850,
'Friction-set brake pedal:1');
#141=(
BOUNDED_CURVE()
B_SPLINE_CURVE(2,(#4882,#4883,#4884),.UNSPECIFIED.,.F.,.F.)
B_SPLINE_CURVE_WITH_KNOTS((3,3),(0.144988513094728,0.791574906712449),
 .UNSPECIFIED.)
CURVE()
GEOMETRIC_REPRESENTATION_ITEM()
RATIONAL_B_SPLINE_CURVE((1.09282032302755,1.26188021535082,1.09282032302931))
REPRESENTATION_ITEM('')
);
#142=(
BOUNDED_CURVE()
B_SPLINE_CURVE(2,(#4886,#4887,#4888),.UNSPECIFIED.,.F.,.F.)
B_SPLINE_CURVE_WITH_KNOTS((3,3),(0.144988513094728,0.791574906712449),
 .UNSPECIFIED.)
CURVE()
GEOMETRIC_REPRESENTATION_ITEM()
RATIONAL_B_SPLINE_CURVE((1.09282032302755,1.26188021535082,1.09282032302931))
REPRESENTATION_ITEM('')
);
#143=(
BOUNDED_CURVE()
B_SPLINE_CURVE(2,(#4890,#4891,#4892),.UNSPECIFIED.,.F.,.F.)
B_SPLINE_CURVE_WITH_KNOTS((3,3),(0.144988513094728,0.791574906712449),
 .UNSPECIFIED.)
CURVE()
GEOMETRIC_REPRESENTATION_ITEM()
RATIONAL_B_SPLINE_CURVE((1.09282032302755,1.26188021535082,1.09282032302931))
REPRESENTATION_ITEM('')
);
#144=(
BOUNDED_CURVE()
B_SPLINE_CURVE(2,(#4894,#4895,#4896),.UNSPECIFIED.,.F.,.F.)
B_SPLINE_CURVE_WITH_KNOTS((3,3),(0.144988513094728,0.791574906712449),
 .UNSPECIFIED.)
CURVE()
GEOMETRIC_REPRESENTATION_ITEM()
RATIONAL_B_SPLINE_CURVE((1.09282032302755,1.26188021535082,1.09282032302931))
REPRESENTATION_ITEM('')
);
#145=(
BOUNDED_CURVE()
B_SPLINE_CURVE(2,(#4898,#4899,#4900),.UNSPECIFIED.,.F.,.F.)
B_SPLINE_CURVE_WITH_KNOTS((3,3),(0.144988513094728,0.791574906712449),
 .UNSPECIFIED.)
CURVE()
GEOMETRIC_REPRESENTATION_ITEM()
RATIONAL_B_SPLINE_CURVE((1.09282032302755,1.26188021535082,1.09282032302931))
REPRESENTATION_ITEM('')
);
#146=(
BOUNDED_CURVE()
B_SPLINE_CURVE(2,(#4901,#4902,#4903),.UNSPECIFIED.,.F.,.F.)
B_SPLINE_CURVE_WITH_KNOTS((3,3),(0.144988513094727,0.791574906712449),
 .UNSPECIFIED.)
CURVE()
GEOMETRIC_REPRESENTATION_ITEM()
RATIONAL_B_SPLINE_CURVE((1.09282032302755,1.26188021535082,1.09282032302931))
REPRESENTATION_ITEM('')
);
#147=(
BOUNDED_CURVE()
B_SPLINE_CURVE(2,(#4934,#4935,#4936),.UNSPECIFIED.,.F.,.F.)
B_SPLINE_CURVE_WITH_KNOTS((3,3),(0.144988513094728,0.791574906712449),
 .UNSPECIFIED.)
CURVE()
GEOMETRIC_REPRESENTATION_ITEM()
RATIONAL_B_SPLINE_CURVE((1.09282032302755,1.26188021535082,1.09282032302931))
REPRESENTATION_ITEM('')
);
#148=(
BOUNDED_CURVE()
B_SPLINE_CURVE(2,(#4938,#4939,#4940),.UNSPECIFIED.,.F.,.F.)
B_SPLINE_CURVE_WITH_KNOTS((3,3),(0.144988513094728,0.791574906712449),
 .UNSPECIFIED.)
CURVE()
GEOMETRIC_REPRESENTATION_ITEM()
RATIONAL_B_SPLINE_CURVE((1.09282032302755,1.26188021535082,1.09282032302931))
REPRESENTATION_ITEM('')
);
#149=(
BOUNDED_CURVE()
B_SPLINE_CURVE(2,(#4945,#4946,#4947),.UNSPECIFIED.,.F.,.F.)
B_SPLINE_CURVE_WITH_KNOTS((3,3),(0.144988513094728,0.791574906712449),
 .UNSPECIFIED.)
CURVE()
GEOMETRIC_REPRESENTATION_ITEM()
RATIONAL_B_SPLINE_CURVE((1.09282032302755,1.26188021535082,1.09282032302931))
REPRESENTATION_ITEM('')
);
#150=(
BOUNDED_CURVE()
B_SPLINE_CURVE(2,(#4949,#4950,#4951),.UNSPECIFIED.,.F.,.F.)
B_SPLINE_CURVE_WITH_KNOTS((3,3),(0.144988513094728,0.791574906712449),
 .UNSPECIFIED.)
CURVE()
GEOMETRIC_REPRESENTATION_ITEM()
RATIONAL_B_SPLINE_CURVE((1.09282032302755,1.26188021535082,1.09282032302931))
REPRESENTATION_ITEM('')
);
#151=(
BOUNDED_CURVE()
B_SPLINE_CURVE(2,(#4953,#4954,#4955),.UNSPECIFIED.,.F.,.F.)
B_SPLINE_CURVE_WITH_KNOTS((3,3),(0.144988513094728,0.791574906712449),
 .UNSPECIFIED.)
CURVE()
GEOMETRIC_REPRESENTATION_ITEM()
RATIONAL_B_SPLINE_CURVE((1.09282032302755,1.26188021535082,1.09282032302931))
REPRESENTATION_ITEM('')
);
#152=(
BOUNDED_CURVE()
B_SPLINE_CURVE(2,(#4956,#4957,#4958),.UNSPECIFIED.,.F.,.F.)
B_SPLINE_CURVE_WITH_KNOTS((3,3),(0.144988513094728,0.791574906712449),
 .UNSPECIFIED.)
CURVE()
GEOMETRIC_REPRESENTATION_ITEM()
RATIONAL_B_SPLINE_CURVE((1.09282032302755,1.26188021535082,1.09282032302931))
REPRESENTATION_ITEM('')
);
#153=(
BOUNDED_CURVE()
B_SPLINE_CURVE(2,(#4965,#4966,#4967),.UNSPECIFIED.,.F.,.F.)
B_SPLINE_CURVE_WITH_KNOTS((3,3),(0.144988513094728,0.791574906712449),
 .UNSPECIFIED.)
CURVE()
GEOMETRIC_REPRESENTATION_ITEM()
RATIONAL_B_SPLINE_CURVE((1.09282032302755,1.26188021535082,1.09282032302931))
REPRESENTATION_ITEM('')
);
#154=(
BOUNDED_CURVE()
B_SPLINE_CURVE(2,(#4969,#4970,#4971),.UNSPECIFIED.,.F.,.F.)
B_SPLINE_CURVE_WITH_KNOTS((3,3),(0.144988513094727,0.791574906712449),
 .UNSPECIFIED.)
CURVE()
GEOMETRIC_REPRESENTATION_ITEM()
RATIONAL_B_SPLINE_CURVE((1.09282032302755,1.26188021535082,1.09282032302931))
REPRESENTATION_ITEM('')
);
#155=(
BOUNDED_CURVE()
B_SPLINE_CURVE(2,(#4973,#4974,#4975),.UNSPECIFIED.,.F.,.F.)
B_SPLINE_CURVE_WITH_KNOTS((3,3),(0.144988513094728,0.791574906712449),
 .UNSPECIFIED.)
CURVE()
GEOMETRIC_REPRESENTATION_ITEM()
RATIONAL_B_SPLINE_CURVE((1.09282032302755,1.26188021535082,1.09282032302931))
REPRESENTATION_ITEM('')
);
#156=(
BOUNDED_CURVE()
B_SPLINE_CURVE(2,(#4977,#4978,#4979),.UNSPECIFIED.,.F.,.F.)
B_SPLINE_CURVE_WITH_KNOTS((3,3),(0.144988513094728,0.791574906712449),
 .UNSPECIFIED.)
CURVE()
GEOMETRIC_REPRESENTATION_ITEM()
RATIONAL_B_SPLINE_CURVE((1.09282032302755,1.26188021535082,1.09282032302931))
REPRESENTATION_ITEM('')
);
#157=(
BOUNDED_CURVE()
B_SPLINE_CURVE(2,(#4981,#4982,#4983),.UNSPECIFIED.,.F.,.F.)
B_SPLINE_CURVE_WITH_KNOTS((3,3),(0.144988513094728,0.791574906712449),
 .UNSPECIFIED.)
CURVE()
GEOMETRIC_REPRESENTATION_ITEM()
RATIONAL_B_SPLINE_CURVE((1.09282032302755,1.26188021535082,1.09282032302931))
REPRESENTATION_ITEM('')
);
#158=(
BOUNDED_CURVE()
B_SPLINE_CURVE(2,(#4984,#4985,#4986),.UNSPECIFIED.,.F.,.F.)
B_SPLINE_CURVE_WITH_KNOTS((3,3),(0.144988513094727,0.791574906712449),
 .UNSPECIFIED.)
CURVE()
GEOMETRIC_REPRESENTATION_ITEM()
RATIONAL_B_SPLINE_CURVE((1.09282032302755,1.26188021535082,1.09282032302931))
REPRESENTATION_ITEM('')
);
#159=CONICAL_SURFACE('',#3306,0.325,0.785398163397448);
#160=CONICAL_SURFACE('',#3310,0.335,0.785398163397448);
#161=CONICAL_SURFACE('',#3314,0.21,0.463647609000806);
#162=CONICAL_SURFACE('',#3330,0.27,0.785398163397448);
#163=CONICAL_SURFACE('',#3333,0.576175134594813,1.0471975511966);
#164=CONICAL_SURFACE('',#3344,0.576175134594813,1.0471975511966);
#165=CONICAL_SURFACE('',#3346,0.576175134594813,1.0471975511966);
#166=CONICAL_SURFACE('',#3400,0.63,0.785398163397448);
#167=CONICAL_SURFACE('',#3407,0.63,0.785398163397448);
#168=CONICAL_SURFACE('',#3420,1.57,0.785398163397449);
#169=CONICAL_SURFACE('',#3424,1.57,0.785398163397449);
#170=ORIENTED_CLOSED_SHELL('',*,#2991,.F.);
#171=BREP_WITH_VOIDS('Body1',#2992,(#170));
#172=SHAPE_REPRESENTATION_RELATIONSHIP('SRR','None',#5810,#189);
#173=SHAPE_REPRESENTATION_RELATIONSHIP('SRR','None',#5811,#190);
#174=SHAPE_REPRESENTATION_RELATIONSHIP('SRR','None',#5812,#191);
#175=SHAPE_REPRESENTATION_RELATIONSHIP('SRR','None',#5813,#192);
#176=SHAPE_REPRESENTATION_RELATIONSHIP('SRR','None',#5814,#193);
#177=SHAPE_REPRESENTATION_RELATIONSHIP('SRR','None',#5815,#194);
#178=SHAPE_REPRESENTATION_RELATIONSHIP('SRR','None',#5816,#195);
#179=SHAPE_REPRESENTATION_RELATIONSHIP('SRR','None',#5817,#196);
#180=SHAPE_REPRESENTATION_RELATIONSHIP('SRR','None',#5819,#197);
#181=SHAPE_REPRESENTATION_RELATIONSHIP('SRR','None',#5821,#198);
#182=SHAPE_REPRESENTATION_RELATIONSHIP('SRR','None',#5822,#199);
#183=SHAPE_REPRESENTATION_RELATIONSHIP('SRR','None',#5823,#200);
#184=SHAPE_REPRESENTATION_RELATIONSHIP('SRR','None',#5824,#201);
#185=SHAPE_REPRESENTATION_RELATIONSHIP('SRR','None',#5825,#202);
#186=SHAPE_REPRESENTATION_RELATIONSHIP('SRR','None',#5826,#203);
#187=SHAPE_REPRESENTATION_RELATIONSHIP('SRR','None',#5828,#204);
#188=SHAPE_REPRESENTATION_RELATIONSHIP('SRR','None',#5829,#205);
#189=ADVANCED_BREP_SHAPE_REPRESENTATION('',(#230),#5714);
#190=ADVANCED_BREP_SHAPE_REPRESENTATION('',(#231),#5715);
#191=ADVANCED_BREP_SHAPE_REPRESENTATION('',(#232),#5716);
#192=ADVANCED_BREP_SHAPE_REPRESENTATION('',(#233),#5717);
#193=ADVANCED_BREP_SHAPE_REPRESENTATION('',(#171),#5718);
#194=ADVANCED_BREP_SHAPE_REPRESENTATION('',(#234),#5719);
#195=ADVANCED_BREP_SHAPE_REPRESENTATION('',(#235),#5720);
#196=ADVANCED_BREP_SHAPE_REPRESENTATION('',(#236),#5721);
#197=ADVANCED_BREP_SHAPE_REPRESENTATION('',(#237),#5723);
#198=ADVANCED_BREP_SHAPE_REPRESENTATION('',(#238),#5725);
#199=ADVANCED_BREP_SHAPE_REPRESENTATION('',(#239),#5726);
#200=ADVANCED_BREP_SHAPE_REPRESENTATION('',(#240,#241,#242,#243,#244,#245,
#246),#5727);
#201=ADVANCED_BREP_SHAPE_REPRESENTATION('',(#247),#5728);
#202=ADVANCED_BREP_SHAPE_REPRESENTATION('',(#248,#249),#5729);
#203=ADVANCED_BREP_SHAPE_REPRESENTATION('',(#250),#5730);
#204=ADVANCED_BREP_SHAPE_REPRESENTATION('',(#251),#5732);
#205=ADVANCED_BREP_SHAPE_REPRESENTATION('',(#252),#5733);
#206=STYLED_ITEM('',(#5984),#230);
#207=STYLED_ITEM('',(#5984),#231);
#208=STYLED_ITEM('',(#5984),#232);
#209=STYLED_ITEM('',(#5984),#233);
#210=STYLED_ITEM('',(#5991),#171);
#211=STYLED_ITEM('',(#5991),#234);
#212=STYLED_ITEM('',(#5991),#235);
#213=STYLED_ITEM('',(#5991),#236);
#214=STYLED_ITEM('',(#5984),#237);
#215=STYLED_ITEM('',(#5984),#238);
#216=STYLED_ITEM('',(#5984),#239);
#217=STYLED_ITEM('',(#5984),#240);
#218=STYLED_ITEM('',(#5984),#241);
#219=STYLED_ITEM('',(#5984),#242);
#220=STYLED_ITEM('',(#5984),#243);
#221=STYLED_ITEM('',(#5984),#244);
#222=STYLED_ITEM('',(#5984),#245);
#223=STYLED_ITEM('',(#5984),#246);
#224=STYLED_ITEM('',(#5984),#247);
#225=STYLED_ITEM('',(#5984),#248);
#226=STYLED_ITEM('',(#5984),#249);
#227=STYLED_ITEM('',(#5984),#250);
#228=STYLED_ITEM('',(#5977),#251);
#229=STYLED_ITEM('',(#5970),#252);
#230=MANIFOLD_SOLID_BREP('Body1',#2987);
#231=MANIFOLD_SOLID_BREP('Body1',#2988);
#232=MANIFOLD_SOLID_BREP('Body1',#2989);
#233=MANIFOLD_SOLID_BREP('Body1',#2990);
#234=MANIFOLD_SOLID_BREP('Body1',#2993);
#235=MANIFOLD_SOLID_BREP('Body1',#2994);
#236=MANIFOLD_SOLID_BREP('Body1',#2995);
#237=MANIFOLD_SOLID_BREP('Body1',#2996);
#238=MANIFOLD_SOLID_BREP('Body1',#2997);
#239=MANIFOLD_SOLID_BREP('Body1',#2998);
#240=MANIFOLD_SOLID_BREP('Body1',#2999);
#241=MANIFOLD_SOLID_BREP('Body2',#3000);
#242=MANIFOLD_SOLID_BREP('Body3',#3001);
#243=MANIFOLD_SOLID_BREP('Body4',#3002);
#244=MANIFOLD_SOLID_BREP('Body5',#3003);
#245=MANIFOLD_SOLID_BREP('Body6',#3004);
#246=MANIFOLD_SOLID_BREP('Body7',#3005);
#247=MANIFOLD_SOLID_BREP('Continuous crown cage',#3006);
#248=MANIFOLD_SOLID_BREP('Body1',#3007);
#249=MANIFOLD_SOLID_BREP('Body2',#3008);
#250=MANIFOLD_SOLID_BREP('Body1',#3009);
#251=MANIFOLD_SOLID_BREP('Body1',#3010);
#252=MANIFOLD_SOLID_BREP('Body1',#3011);
#253=CYLINDRICAL_SURFACE('',#3213,0.325);
#254=CYLINDRICAL_SURFACE('',#3216,0.325);
#255=CYLINDRICAL_SURFACE('',#3225,0.6);
#256=CYLINDRICAL_SURFACE('',#3228,0.6);
#257=CYLINDRICAL_SURFACE('',#3243,0.425);
#258=CYLINDRICAL_SURFACE('',#3246,0.425);
#259=CYLINDRICAL_SURFACE('',#3249,0.425);
#260=CYLINDRICAL_SURFACE('',#3252,0.425);
#261=CYLINDRICAL_SURFACE('',#3262,0.165);
#262=CYLINDRICAL_SURFACE('',#3269,0.9);
#263=CYLINDRICAL_SURFACE('',#3272,0.6);
#264=CYLINDRICAL_SURFACE('',#3276,0.605);
#265=CYLINDRICAL_SURFACE('',#3279,0.8);
#266=CYLINDRICAL_SURFACE('',#3285,0.225);
#267=CYLINDRICAL_SURFACE('',#3288,0.8);
#268=CYLINDRICAL_SURFACE('',#3308,0.35);
#269=CYLINDRICAL_SURFACE('',#3316,0.1954);
#270=CYLINDRICAL_SURFACE('',#3318,0.32);
#271=CYLINDRICAL_SURFACE('',#3321,0.6);
#272=CYLINDRICAL_SURFACE('',#3327,0.2942);
#273=CYLINDRICAL_SURFACE('',#3351,0.25175);
#274=CYLINDRICAL_SURFACE('',#3371,1.6);
#275=CYLINDRICAL_SURFACE('',#3376,1.6);
#276=CYLINDRICAL_SURFACE('',#3381,0.62);
#277=CYLINDRICAL_SURFACE('',#3382,3.75);
#278=CYLINDRICAL_SURFACE('',#3395,1.070235);
#279=CYLINDRICAL_SURFACE('',#3397,0.6);
#280=CYLINDRICAL_SURFACE('',#3403,1.070235);
#281=CYLINDRICAL_SURFACE('',#3415,1.129765);
#282=CYLINDRICAL_SURFACE('',#3422,1.6);
#283=CYLINDRICAL_SURFACE('',#3427,1.129765);
#284=CYLINDRICAL_SURFACE('',#3447,1.123812);
#285=CYLINDRICAL_SURFACE('',#3483,1.076188);
#286=CYLINDRICAL_SURFACE('',#3497,1.119765);
#287=CYLINDRICAL_SURFACE('',#3501,1.085235);
#288=CYLINDRICAL_SURFACE('',#3505,1.119765);
#289=CYLINDRICAL_SURFACE('',#3509,1.085235);
#290=CYLINDRICAL_SURFACE('',#3516,1.2);
#291=CYLINDRICAL_SURFACE('',#3519,1.6);
#292=CYLINDRICAL_SURFACE('',#3531,0.325);
#293=CYLINDRICAL_SURFACE('',#3540,0.6);
#294=CYLINDRICAL_SURFACE('',#3548,0.6);
#295=FACE_BOUND('',#661,.T.);
#296=FACE_BOUND('',#667,.T.);
#297=FACE_BOUND('',#671,.T.);
#298=FACE_BOUND('',#675,.T.);
#299=FACE_BOUND('',#699,.T.);
#300=FACE_BOUND('',#700,.T.);
#301=FACE_BOUND('',#701,.T.);
#302=FACE_BOUND('',#702,.T.);
#303=FACE_BOUND('',#703,.T.);
#304=FACE_BOUND('',#705,.T.);
#305=FACE_BOUND('',#706,.T.);
#306=FACE_BOUND('',#707,.T.);
#307=FACE_BOUND('',#708,.T.);
#308=FACE_BOUND('',#709,.T.);
#309=FACE_BOUND('',#710,.T.);
#310=FACE_BOUND('',#711,.T.);
#311=FACE_BOUND('',#715,.T.);
#312=FACE_BOUND('',#720,.T.);
#313=FACE_BOUND('',#724,.T.);
#314=FACE_BOUND('',#726,.T.);
#315=FACE_BOUND('',#730,.T.);
#316=FACE_BOUND('',#732,.T.);
#317=FACE_BOUND('',#747,.T.);
#318=FACE_BOUND('',#753,.T.);
#319=FACE_BOUND('',#755,.T.);
#320=FACE_BOUND('',#768,.T.);
#321=FACE_BOUND('',#779,.T.);
#322=FACE_BOUND('',#781,.T.);
#323=FACE_BOUND('',#784,.T.);
#324=FACE_BOUND('',#787,.T.);
#325=FACE_BOUND('',#791,.T.);
#326=FACE_BOUND('',#793,.T.);
#327=FACE_BOUND('',#799,.T.);
#328=FACE_BOUND('',#802,.T.);
#329=FACE_BOUND('',#807,.T.);
#330=FACE_BOUND('',#812,.T.);
#331=FACE_BOUND('',#837,.T.);
#332=FACE_BOUND('',#840,.T.);
#333=FACE_BOUND('',#843,.T.);
#334=FACE_BOUND('',#846,.T.);
#335=FACE_BOUND('',#849,.T.);
#336=FACE_BOUND('',#854,.T.);
#337=FACE_BOUND('',#856,.T.);
#338=FACE_BOUND('',#862,.T.);
#339=FACE_BOUND('',#869,.T.);
#340=CIRCLE('',#3210,0.325);
#341=CIRCLE('',#3214,0.325);
#342=CIRCLE('',#3215,0.325);
#343=CIRCLE('',#3217,0.325);
#344=CIRCLE('',#3226,0.6);
#345=CIRCLE('',#3227,0.6);
#346=CIRCLE('',#3229,0.6);
#347=CIRCLE('',#3230,0.6);
#348=CIRCLE('',#3244,0.425);
#349=CIRCLE('',#3245,0.425);
#350=CIRCLE('',#3247,0.425);
#351=CIRCLE('',#3248,0.425);
#352=CIRCLE('',#3250,0.425);
#353=CIRCLE('',#3251,0.425);
#354=CIRCLE('',#3253,0.425);
#355=CIRCLE('',#3254,0.425);
#356=CIRCLE('',#3263,0.165);
#357=CIRCLE('',#3264,0.165);
#358=CIRCLE('',#3267,0.9);
#359=CIRCLE('',#3268,0.6);
#360=CIRCLE('',#3270,0.9);
#361=CIRCLE('',#3273,0.6);
#362=CIRCLE('',#3277,0.605);
#363=CIRCLE('',#3278,0.605);
#364=CIRCLE('',#3280,0.8);
#365=CIRCLE('',#3281,0.8);
#366=CIRCLE('',#3286,0.225);
#367=CIRCLE('',#3287,0.225);
#368=CIRCLE('',#3289,0.8);
#369=CIRCLE('',#3290,0.8);
#370=CIRCLE('',#3303,0.1954);
#371=CIRCLE('',#3305,0.3);
#372=CIRCLE('',#3307,0.35);
#373=CIRCLE('',#3309,0.35);
#374=CIRCLE('',#3311,0.32);
#375=CIRCLE('',#3313,0.22);
#376=CIRCLE('',#3315,0.1954);
#377=CIRCLE('',#3319,0.32);
#378=CIRCLE('',#3320,0.32);
#379=CIRCLE('',#3322,0.6);
#380=CIRCLE('',#3323,0.6);
#381=CIRCLE('',#3328,0.2942);
#382=CIRCLE('',#3329,0.2942);
#383=CIRCLE('',#3331,0.24);
#384=CIRCLE('',#3334,0.475);
#385=CIRCLE('',#3345,0.475);
#386=CIRCLE('',#3347,0.475);
#387=CIRCLE('',#3352,0.25175);
#388=CIRCLE('',#3353,0.25175);
#389=CIRCLE('',#3372,1.6);
#390=CIRCLE('',#3373,1.6);
#391=CIRCLE('',#3375,0.62);
#392=CIRCLE('',#3377,1.6);
#393=CIRCLE('',#3378,1.6);
#394=CIRCLE('',#3380,0.62);
#395=CIRCLE('',#3383,3.75);
#396=CIRCLE('',#3384,3.75);
#397=CIRCLE('',#3390,1.070235);
#398=CIRCLE('',#3391,1.070235);
#399=CIRCLE('',#3392,0.309556);
#400=CIRCLE('',#3393,1.070235);
#401=CIRCLE('',#3394,1.070235);
#402=CIRCLE('',#3396,1.070235);
#403=CIRCLE('',#3398,0.6);
#404=CIRCLE('',#3399,0.6);
#405=CIRCLE('',#3401,0.66);
#406=CIRCLE('',#3404,1.070235);
#407=CIRCLE('',#3406,0.66);
#408=CIRCLE('',#3410,1.129765);
#409=CIRCLE('',#3411,1.129765);
#410=CIRCLE('',#3412,0.309556);
#411=CIRCLE('',#3413,1.129765);
#412=CIRCLE('',#3414,1.129765);
#413=CIRCLE('',#3416,1.129765);
#414=CIRCLE('',#3418,1.54);
#415=CIRCLE('',#3419,1.129765);
#416=CIRCLE('',#3421,1.6);
#417=CIRCLE('',#3423,1.6);
#418=CIRCLE('',#3425,1.54);
#419=CIRCLE('',#3430,0.29765);
#420=CIRCLE('',#3432,0.29765);
#421=CIRCLE('',#3434,0.29765);
#422=CIRCLE('',#3436,0.29765);
#423=CIRCLE('',#3438,0.29765);
#424=CIRCLE('',#3440,0.29765);
#425=CIRCLE('',#3442,0.29765);
#426=CIRCLE('',#3445,0.303778037777585);
#427=CIRCLE('',#3446,0.303778037777585);
#428=CIRCLE('',#3448,1.123812);
#429=CIRCLE('',#3449,1.123812);
#430=CIRCLE('',#3450,1.123812);
#431=CIRCLE('',#3451,1.123812);
#432=CIRCLE('',#3452,1.123812);
#433=CIRCLE('',#3453,1.123812);
#434=CIRCLE('',#3454,1.123812);
#435=CIRCLE('',#3455,1.123812);
#436=CIRCLE('',#3456,1.123812);
#437=CIRCLE('',#3458,1.076188);
#438=CIRCLE('',#3459,0.303778037777585);
#439=CIRCLE('',#3461,0.303778037777585);
#440=CIRCLE('',#3463,1.076188);
#441=CIRCLE('',#3464,0.303778037777585);
#442=CIRCLE('',#3466,0.303778037777585);
#443=CIRCLE('',#3468,1.076188);
#444=CIRCLE('',#3469,1.076188);
#445=CIRCLE('',#3470,0.303778037777585);
#446=CIRCLE('',#3472,0.303778037777585);
#447=CIRCLE('',#3474,1.076188);
#448=CIRCLE('',#3475,0.303778037777585);
#449=CIRCLE('',#3477,0.303778037777585);
#450=CIRCLE('',#3479,1.076188);
#451=CIRCLE('',#3480,0.303778037777585);
#452=CIRCLE('',#3482,0.303778037777585);
#453=CIRCLE('',#3484,1.076188);
#454=CIRCLE('',#3485,1.076188);
#455=CIRCLE('',#3486,1.076188);
#456=CIRCLE('',#3488,0.303778037777585);
#457=CIRCLE('',#3490,0.303778037777585);
#458=CIRCLE('',#3495,1.119765);
#459=CIRCLE('',#3496,1.085235);
#460=CIRCLE('',#3498,1.119765);
#461=CIRCLE('',#3500,1.085235);
#462=CIRCLE('',#3503,1.119765);
#463=CIRCLE('',#3504,1.085235);
#464=CIRCLE('',#3506,1.119765);
#465=CIRCLE('',#3508,1.085235);
#466=CIRCLE('',#3517,1.2);
#467=CIRCLE('',#3518,1.2);
#468=CIRCLE('',#3520,1.6);
#469=CIRCLE('',#3521,1.6);
#470=CIRCLE('',#3532,0.325);
#471=CIRCLE('',#3533,0.325);
#472=CIRCLE('',#3538,0.6);
#473=CIRCLE('',#3539,0.6);
#474=CIRCLE('',#3541,0.6);
#475=CIRCLE('',#3547,0.6);
#476=FACE_OUTER_BOUND('',#654,.T.);
#477=FACE_OUTER_BOUND('',#655,.T.);
#478=FACE_OUTER_BOUND('',#656,.T.);
#479=FACE_OUTER_BOUND('',#657,.T.);
#480=FACE_OUTER_BOUND('',#658,.T.);
#481=FACE_OUTER_BOUND('',#659,.T.);
#482=FACE_OUTER_BOUND('',#660,.T.);
#483=FACE_OUTER_BOUND('',#662,.T.);
#484=FACE_OUTER_BOUND('',#663,.T.);
#485=FACE_OUTER_BOUND('',#664,.T.);
#486=FACE_OUTER_BOUND('',#665,.T.);
#487=FACE_OUTER_BOUND('',#666,.T.);
#488=FACE_OUTER_BOUND('',#668,.T.);
#489=FACE_OUTER_BOUND('',#669,.T.);
#490=FACE_OUTER_BOUND('',#670,.T.);
#491=FACE_OUTER_BOUND('',#672,.T.);
#492=FACE_OUTER_BOUND('',#673,.T.);
#493=FACE_OUTER_BOUND('',#674,.T.);
#494=FACE_OUTER_BOUND('',#676,.T.);
#495=FACE_OUTER_BOUND('',#677,.T.);
#496=FACE_OUTER_BOUND('',#678,.T.);
#497=FACE_OUTER_BOUND('',#679,.T.);
#498=FACE_OUTER_BOUND('',#680,.T.);
#499=FACE_OUTER_BOUND('',#681,.T.);
#500=FACE_OUTER_BOUND('',#682,.T.);
#501=FACE_OUTER_BOUND('',#683,.T.);
#502=FACE_OUTER_BOUND('',#684,.T.);
#503=FACE_OUTER_BOUND('',#685,.T.);
#504=FACE_OUTER_BOUND('',#686,.T.);
#505=FACE_OUTER_BOUND('',#687,.T.);
#506=FACE_OUTER_BOUND('',#688,.T.);
#507=FACE_OUTER_BOUND('',#689,.T.);
#508=FACE_OUTER_BOUND('',#690,.T.);
#509=FACE_OUTER_BOUND('',#691,.T.);
#510=FACE_OUTER_BOUND('',#692,.T.);
#511=FACE_OUTER_BOUND('',#693,.T.);
#512=FACE_OUTER_BOUND('',#694,.T.);
#513=FACE_OUTER_BOUND('',#695,.T.);
#514=FACE_OUTER_BOUND('',#696,.T.);
#515=FACE_OUTER_BOUND('',#697,.T.);
#516=FACE_OUTER_BOUND('',#698,.T.);
#517=FACE_OUTER_BOUND('',#704,.T.);
#518=FACE_OUTER_BOUND('',#712,.T.);
#519=FACE_OUTER_BOUND('',#713,.T.);
#520=FACE_OUTER_BOUND('',#714,.T.);
#521=FACE_OUTER_BOUND('',#716,.T.);
#522=FACE_OUTER_BOUND('',#717,.T.);
#523=FACE_OUTER_BOUND('',#718,.T.);
#524=FACE_OUTER_BOUND('',#719,.T.);
#525=FACE_OUTER_BOUND('',#721,.T.);
#526=FACE_OUTER_BOUND('',#722,.T.);
#527=FACE_OUTER_BOUND('',#723,.T.);
#528=FACE_OUTER_BOUND('',#725,.T.);
#529=FACE_OUTER_BOUND('',#727,.T.);
#530=FACE_OUTER_BOUND('',#728,.T.);
#531=FACE_OUTER_BOUND('',#729,.T.);
#532=FACE_OUTER_BOUND('',#731,.T.);
#533=FACE_OUTER_BOUND('',#733,.T.);
#534=FACE_OUTER_BOUND('',#734,.T.);
#535=FACE_OUTER_BOUND('',#735,.T.);
#536=FACE_OUTER_BOUND('',#736,.T.);
#537=FACE_OUTER_BOUND('',#737,.T.);
#538=FACE_OUTER_BOUND('',#738,.T.);
#539=FACE_OUTER_BOUND('',#739,.T.);
#540=FACE_OUTER_BOUND('',#740,.T.);
#541=FACE_OUTER_BOUND('',#741,.T.);
#542=FACE_OUTER_BOUND('',#742,.T.);
#543=FACE_OUTER_BOUND('',#743,.T.);
#544=FACE_OUTER_BOUND('',#744,.T.);
#545=FACE_OUTER_BOUND('',#745,.T.);
#546=FACE_OUTER_BOUND('',#746,.T.);
#547=FACE_OUTER_BOUND('',#748,.T.);
#548=FACE_OUTER_BOUND('',#749,.T.);
#549=FACE_OUTER_BOUND('',#750,.T.);
#550=FACE_OUTER_BOUND('',#751,.T.);
#551=FACE_OUTER_BOUND('',#752,.T.);
#552=FACE_OUTER_BOUND('',#754,.T.);
#553=FACE_OUTER_BOUND('',#756,.T.);
#554=FACE_OUTER_BOUND('',#757,.T.);
#555=FACE_OUTER_BOUND('',#758,.T.);
#556=FACE_OUTER_BOUND('',#759,.T.);
#557=FACE_OUTER_BOUND('',#760,.T.);
#558=FACE_OUTER_BOUND('',#761,.T.);
#559=FACE_OUTER_BOUND('',#762,.T.);
#560=FACE_OUTER_BOUND('',#763,.T.);
#561=FACE_OUTER_BOUND('',#764,.T.);
#562=FACE_OUTER_BOUND('',#765,.T.);
#563=FACE_OUTER_BOUND('',#766,.T.);
#564=FACE_OUTER_BOUND('',#767,.T.);
#565=FACE_OUTER_BOUND('',#769,.T.);
#566=FACE_OUTER_BOUND('',#770,.T.);
#567=FACE_OUTER_BOUND('',#771,.T.);
#568=FACE_OUTER_BOUND('',#772,.T.);
#569=FACE_OUTER_BOUND('',#773,.T.);
#570=FACE_OUTER_BOUND('',#774,.T.);
#571=FACE_OUTER_BOUND('',#775,.T.);
#572=FACE_OUTER_BOUND('',#776,.T.);
#573=FACE_OUTER_BOUND('',#777,.T.);
#574=FACE_OUTER_BOUND('',#778,.T.);
#575=FACE_OUTER_BOUND('',#780,.T.);
#576=FACE_OUTER_BOUND('',#782,.T.);
#577=FACE_OUTER_BOUND('',#783,.T.);
#578=FACE_OUTER_BOUND('',#785,.T.);
#579=FACE_OUTER_BOUND('',#786,.T.);
#580=FACE_OUTER_BOUND('',#788,.T.);
#581=FACE_OUTER_BOUND('',#789,.T.);
#582=FACE_OUTER_BOUND('',#790,.T.);
#583=FACE_OUTER_BOUND('',#792,.T.);
#584=FACE_OUTER_BOUND('',#794,.T.);
#585=FACE_OUTER_BOUND('',#795,.T.);
#586=FACE_OUTER_BOUND('',#796,.T.);
#587=FACE_OUTER_BOUND('',#797,.T.);
#588=FACE_OUTER_BOUND('',#798,.T.);
#589=FACE_OUTER_BOUND('',#800,.T.);
#590=FACE_OUTER_BOUND('',#801,.T.);
#591=FACE_OUTER_BOUND('',#803,.T.);
#592=FACE_OUTER_BOUND('',#804,.T.);
#593=FACE_OUTER_BOUND('',#805,.T.);
#594=FACE_OUTER_BOUND('',#806,.T.);
#595=FACE_OUTER_BOUND('',#808,.T.);
#596=FACE_OUTER_BOUND('',#809,.T.);
#597=FACE_OUTER_BOUND('',#810,.T.);
#598=FACE_OUTER_BOUND('',#811,.T.);
#599=FACE_OUTER_BOUND('',#813,.T.);
#600=FACE_OUTER_BOUND('',#814,.T.);
#601=FACE_OUTER_BOUND('',#815,.T.);
#602=FACE_OUTER_BOUND('',#816,.T.);
#603=FACE_OUTER_BOUND('',#817,.T.);
#604=FACE_OUTER_BOUND('',#818,.T.);
#605=FACE_OUTER_BOUND('',#819,.T.);
#606=FACE_OUTER_BOUND('',#820,.T.);
#607=FACE_OUTER_BOUND('',#821,.T.);
#608=FACE_OUTER_BOUND('',#822,.T.);
#609=FACE_OUTER_BOUND('',#823,.T.);
#610=FACE_OUTER_BOUND('',#824,.T.);
#611=FACE_OUTER_BOUND('',#825,.T.);
#612=FACE_OUTER_BOUND('',#826,.T.);
#613=FACE_OUTER_BOUND('',#827,.T.);
#614=FACE_OUTER_BOUND('',#828,.T.);
#615=FACE_OUTER_BOUND('',#829,.T.);
#616=FACE_OUTER_BOUND('',#830,.T.);
#617=FACE_OUTER_BOUND('',#831,.T.);
#618=FACE_OUTER_BOUND('',#832,.T.);
#619=FACE_OUTER_BOUND('',#833,.T.);
#620=FACE_OUTER_BOUND('',#834,.T.);
#621=FACE_OUTER_BOUND('',#835,.T.);
#622=FACE_OUTER_BOUND('',#836,.T.);
#623=FACE_OUTER_BOUND('',#838,.T.);
#624=FACE_OUTER_BOUND('',#839,.T.);
#625=FACE_OUTER_BOUND('',#841,.T.);
#626=FACE_OUTER_BOUND('',#842,.T.);
#627=FACE_OUTER_BOUND('',#844,.T.);
#628=FACE_OUTER_BOUND('',#845,.T.);
#629=FACE_OUTER_BOUND('',#847,.T.);
#630=FACE_OUTER_BOUND('',#848,.T.);
#631=FACE_OUTER_BOUND('',#850,.T.);
#632=FACE_OUTER_BOUND('',#851,.T.);
#633=FACE_OUTER_BOUND('',#852,.T.);
#634=FACE_OUTER_BOUND('',#853,.T.);
#635=FACE_OUTER_BOUND('',#855,.T.);
#636=FACE_OUTER_BOUND('',#857,.T.);
#637=FACE_OUTER_BOUND('',#858,.T.);
#638=FACE_OUTER_BOUND('',#859,.T.);
#639=FACE_OUTER_BOUND('',#860,.T.);
#640=FACE_OUTER_BOUND('',#861,.T.);
#641=FACE_OUTER_BOUND('',#863,.T.);
#642=FACE_OUTER_BOUND('',#864,.T.);
#643=FACE_OUTER_BOUND('',#865,.T.);
#644=FACE_OUTER_BOUND('',#866,.T.);
#645=FACE_OUTER_BOUND('',#867,.T.);
#646=FACE_OUTER_BOUND('',#868,.T.);
#647=FACE_OUTER_BOUND('',#870,.T.);
#648=FACE_OUTER_BOUND('',#871,.T.);
#649=FACE_OUTER_BOUND('',#872,.T.);
#650=FACE_OUTER_BOUND('',#873,.T.);
#651=FACE_OUTER_BOUND('',#874,.T.);
#652=FACE_OUTER_BOUND('',#875,.T.);
#653=FACE_OUTER_BOUND('',#876,.T.);
#654=EDGE_LOOP('',(#1940,#1941,#1942,#1943));
#655=EDGE_LOOP('',(#1944,#1945,#1946,#1947,#1948,#1949,#1950,#1951));
#656=EDGE_LOOP('',(#1952,#1953,#1954,#1955));
#657=EDGE_LOOP('',(#1956,#1957,#1958,#1959));
#658=EDGE_LOOP('',(#1960,#1961,#1962,#1963,#1964,#1965,#1966,#1967));
#659=EDGE_LOOP('',(#1968,#1969,#1970,#1971));
#660=EDGE_LOOP('',(#1972,#1973,#1974,#1975));
#661=EDGE_LOOP('',(#1976));
#662=EDGE_LOOP('',(#1977,#1978,#1979,#1980,#1981,#1982));
#663=EDGE_LOOP('',(#1983,#1984,#1985,#1986,#1987,#1988));
#664=EDGE_LOOP('',(#1989,#1990,#1991,#1992));
#665=EDGE_LOOP('',(#1993,#1994,#1995,#1996));
#666=EDGE_LOOP('',(#1997,#1998,#1999,#2000));
#667=EDGE_LOOP('',(#2001));
#668=EDGE_LOOP('',(#2002,#2003,#2004,#2005,#2006,#2007));
#669=EDGE_LOOP('',(#2008,#2009,#2010,#2011));
#670=EDGE_LOOP('',(#2012,#2013,#2014,#2015));
#671=EDGE_LOOP('',(#2016));
#672=EDGE_LOOP('',(#2017,#2018,#2019,#2020,#2021,#2022));
#673=EDGE_LOOP('',(#2023,#2024,#2025,#2026));
#674=EDGE_LOOP('',(#2027,#2028,#2029,#2030));
#675=EDGE_LOOP('',(#2031));
#676=EDGE_LOOP('',(#2032,#2033,#2034,#2035));
#677=EDGE_LOOP('',(#2036,#2037,#2038,#2039));
#678=EDGE_LOOP('',(#2040,#2041,#2042,#2043,#2044,#2045));
#679=EDGE_LOOP('',(#2046,#2047,#2048,#2049));
#680=EDGE_LOOP('',(#2050,#2051,#2052,#2053,#2054,#2055));
#681=EDGE_LOOP('',(#2056,#2057,#2058,#2059));
#682=EDGE_LOOP('',(#2060,#2061,#2062,#2063,#2064,#2065));
#683=EDGE_LOOP('',(#2066,#2067,#2068,#2069));
#684=EDGE_LOOP('',(#2070,#2071,#2072,#2073));
#685=EDGE_LOOP('',(#2074,#2075,#2076,#2077));
#686=EDGE_LOOP('',(#2078,#2079,#2080,#2081,#2082,#2083));
#687=EDGE_LOOP('',(#2084,#2085,#2086,#2087));
#688=EDGE_LOOP('',(#2088,#2089,#2090,#2091));
#689=EDGE_LOOP('',(#2092,#2093,#2094,#2095));
#690=EDGE_LOOP('',(#2096,#2097,#2098,#2099));
#691=EDGE_LOOP('',(#2100,#2101,#2102,#2103));
#692=EDGE_LOOP('',(#2104,#2105,#2106,#2107));
#693=EDGE_LOOP('',(#2108,#2109,#2110,#2111));
#694=EDGE_LOOP('',(#2112,#2113,#2114,#2115));
#695=EDGE_LOOP('',(#2116,#2117,#2118,#2119));
#696=EDGE_LOOP('',(#2120,#2121,#2122,#2123));
#697=EDGE_LOOP('',(#2124,#2125,#2126,#2127));
#698=EDGE_LOOP('',(#2128,#2129,#2130,#2131));
#699=EDGE_LOOP('',(#2132,#2133,#2134,#2135));
#700=EDGE_LOOP('',(#2136));
#701=EDGE_LOOP('',(#2137));
#702=EDGE_LOOP('',(#2138));
#703=EDGE_LOOP('',(#2139));
#704=EDGE_LOOP('',(#2140,#2141,#2142,#2143));
#705=EDGE_LOOP('',(#2144,#2145,#2146,#2147,#2148,#2149,#2150,#2151,#2152,
#2153,#2154,#2155));
#706=EDGE_LOOP('',(#2156));
#707=EDGE_LOOP('',(#2157));
#708=EDGE_LOOP('',(#2158));
#709=EDGE_LOOP('',(#2159));
#710=EDGE_LOOP('',(#2160,#2161,#2162,#2163));
#711=EDGE_LOOP('',(#2164,#2165,#2166,#2167));
#712=EDGE_LOOP('',(#2168,#2169,#2170,#2171));
#713=EDGE_LOOP('',(#2172));
#714=EDGE_LOOP('',(#2173));
#715=EDGE_LOOP('',(#2174));
#716=EDGE_LOOP('',(#2175,#2176,#2177,#2178));
#717=EDGE_LOOP('',(#2179));
#718=EDGE_LOOP('',(#2180,#2181,#2182,#2183));
#719=EDGE_LOOP('',(#2184));
#720=EDGE_LOOP('',(#2185));
#721=EDGE_LOOP('',(#2186,#2187,#2188,#2189));
#722=EDGE_LOOP('',(#2190,#2191,#2192,#2193));
#723=EDGE_LOOP('',(#2194));
#724=EDGE_LOOP('',(#2195));
#725=EDGE_LOOP('',(#2196));
#726=EDGE_LOOP('',(#2197));
#727=EDGE_LOOP('',(#2198,#2199,#2200,#2201));
#728=EDGE_LOOP('',(#2202,#2203,#2204,#2205));
#729=EDGE_LOOP('',(#2206));
#730=EDGE_LOOP('',(#2207));
#731=EDGE_LOOP('',(#2208));
#732=EDGE_LOOP('',(#2209));
#733=EDGE_LOOP('',(#2210,#2211,#2212,#2213));
#734=EDGE_LOOP('',(#2214,#2215,#2216,#2217));
#735=EDGE_LOOP('',(#2218,#2219,#2220,#2221));
#736=EDGE_LOOP('',(#2222,#2223,#2224,#2225));
#737=EDGE_LOOP('',(#2226,#2227,#2228,#2229));
#738=EDGE_LOOP('',(#2230,#2231,#2232,#2233));
#739=EDGE_LOOP('',(#2234,#2235,#2236,#2237,#2238,#2239));
#740=EDGE_LOOP('',(#2240,#2241,#2242,#2243,#2244,#2245));
#741=EDGE_LOOP('',(#2246));
#742=EDGE_LOOP('',(#2247));
#743=EDGE_LOOP('',(#2248,#2249,#2250,#2251));
#744=EDGE_LOOP('',(#2252,#2253,#2254,#2255));
#745=EDGE_LOOP('',(#2256,#2257,#2258,#2259));
#746=EDGE_LOOP('',(#2260));
#747=EDGE_LOOP('',(#2261));
#748=EDGE_LOOP('',(#2262,#2263,#2264,#2265));
#749=EDGE_LOOP('',(#2266,#2267,#2268,#2269));
#750=EDGE_LOOP('',(#2270,#2271,#2272,#2273));
#751=EDGE_LOOP('',(#2274,#2275,#2276,#2277));
#752=EDGE_LOOP('',(#2278));
#753=EDGE_LOOP('',(#2279));
#754=EDGE_LOOP('',(#2280));
#755=EDGE_LOOP('',(#2281));
#756=EDGE_LOOP('',(#2282,#2283,#2284,#2285));
#757=EDGE_LOOP('',(#2286,#2287,#2288,#2289));
#758=EDGE_LOOP('',(#2290));
#759=EDGE_LOOP('',(#2291,#2292,#2293,#2294,#2295,#2296,#2297,#2298,#2299));
#760=EDGE_LOOP('',(#2300,#2301,#2302,#2303));
#761=EDGE_LOOP('',(#2304,#2305,#2306,#2307));
#762=EDGE_LOOP('',(#2308,#2309,#2310,#2311));
#763=EDGE_LOOP('',(#2312,#2313,#2314,#2315));
#764=EDGE_LOOP('',(#2316,#2317,#2318,#2319));
#765=EDGE_LOOP('',(#2320,#2321,#2322,#2323));
#766=EDGE_LOOP('',(#2324));
#767=EDGE_LOOP('',(#2325,#2326,#2327,#2328,#2329,#2330));
#768=EDGE_LOOP('',(#2331));
#769=EDGE_LOOP('',(#2332,#2333,#2334,#2335,#2336,#2337,#2338,#2339,#2340));
#770=EDGE_LOOP('',(#2341,#2342,#2343,#2344,#2345,#2346,#2347,#2348,#2349));
#771=EDGE_LOOP('',(#2350,#2351,#2352,#2353));
#772=EDGE_LOOP('',(#2354,#2355,#2356,#2357));
#773=EDGE_LOOP('',(#2358,#2359,#2360,#2361));
#774=EDGE_LOOP('',(#2362,#2363,#2364,#2365));
#775=EDGE_LOOP('',(#2366,#2367,#2368,#2369));
#776=EDGE_LOOP('',(#2370,#2371,#2372,#2373));
#777=EDGE_LOOP('',(#2374,#2375,#2376,#2377));
#778=EDGE_LOOP('',(#2378));
#779=EDGE_LOOP('',(#2379));
#780=EDGE_LOOP('',(#2380));
#781=EDGE_LOOP('',(#2381));
#782=EDGE_LOOP('',(#2382,#2383,#2384,#2385));
#783=EDGE_LOOP('',(#2386));
#784=EDGE_LOOP('',(#2387));
#785=EDGE_LOOP('',(#2388,#2389,#2390,#2391));
#786=EDGE_LOOP('',(#2392));
#787=EDGE_LOOP('',(#2393));
#788=EDGE_LOOP('',(#2394,#2395,#2396,#2397));
#789=EDGE_LOOP('',(#2398,#2399,#2400,#2401));
#790=EDGE_LOOP('',(#2402));
#791=EDGE_LOOP('',(#2403));
#792=EDGE_LOOP('',(#2404));
#793=EDGE_LOOP('',(#2405));
#794=EDGE_LOOP('',(#2406,#2407,#2408,#2409,#2410,#2411));
#795=EDGE_LOOP('',(#2412,#2413,#2414,#2415,#2416));
#796=EDGE_LOOP('',(#2417,#2418,#2419,#2420));
#797=EDGE_LOOP('',(#2421,#2422,#2423,#2424));
#798=EDGE_LOOP('',(#2425));
#799=EDGE_LOOP('',(#2426));
#800=EDGE_LOOP('',(#2427,#2428,#2429,#2430,#2431));
#801=EDGE_LOOP('',(#2432));
#802=EDGE_LOOP('',(#2433));
#803=EDGE_LOOP('',(#2434,#2435,#2436,#2437));
#804=EDGE_LOOP('',(#2438,#2439,#2440,#2441,#2442,#2443));
#805=EDGE_LOOP('',(#2444,#2445,#2446,#2447,#2448));
#806=EDGE_LOOP('',(#2449));
#807=EDGE_LOOP('',(#2450));
#808=EDGE_LOOP('',(#2451,#2452,#2453,#2454));
#809=EDGE_LOOP('',(#2455,#2456,#2457,#2458));
#810=EDGE_LOOP('',(#2459,#2460,#2461,#2462));
#811=EDGE_LOOP('',(#2463));
#812=EDGE_LOOP('',(#2464));
#813=EDGE_LOOP('',(#2465,#2466,#2467,#2468,#2469));
#814=EDGE_LOOP('',(#2470,#2471));
#815=EDGE_LOOP('',(#2472,#2473));
#816=EDGE_LOOP('',(#2474,#2475));
#817=EDGE_LOOP('',(#2476,#2477));
#818=EDGE_LOOP('',(#2478,#2479));
#819=EDGE_LOOP('',(#2480,#2481));
#820=EDGE_LOOP('',(#2482,#2483));
#821=EDGE_LOOP('',(#2484,#2485,#2486,#2487));
#822=EDGE_LOOP('',(#2488,#2489,#2490,#2491,#2492,#2493,#2494,#2495,#2496,
#2497,#2498,#2499,#2500,#2501,#2502,#2503,#2504,#2505));
#823=EDGE_LOOP('',(#2506,#2507,#2508,#2509));
#824=EDGE_LOOP('',(#2510,#2511,#2512,#2513));
#825=EDGE_LOOP('',(#2514,#2515,#2516,#2517));
#826=EDGE_LOOP('',(#2518,#2519,#2520,#2521));
#827=EDGE_LOOP('',(#2522,#2523,#2524,#2525,#2526,#2527));
#828=EDGE_LOOP('',(#2528,#2529,#2530,#2531));
#829=EDGE_LOOP('',(#2532,#2533,#2534,#2535));
#830=EDGE_LOOP('',(#2536,#2537,#2538,#2539));
#831=EDGE_LOOP('',(#2540,#2541,#2542,#2543));
#832=EDGE_LOOP('',(#2544,#2545,#2546,#2547));
#833=EDGE_LOOP('',(#2548,#2549,#2550,#2551,#2552,#2553,#2554,#2555,#2556,
#2557,#2558,#2559,#2560,#2561,#2562,#2563,#2564,#2565));
#834=EDGE_LOOP('',(#2566,#2567,#2568,#2569));
#835=EDGE_LOOP('',(#2570,#2571,#2572,#2573));
#836=EDGE_LOOP('',(#2574));
#837=EDGE_LOOP('',(#2575));
#838=EDGE_LOOP('',(#2576,#2577,#2578,#2579));
#839=EDGE_LOOP('',(#2580));
#840=EDGE_LOOP('',(#2581));
#841=EDGE_LOOP('',(#2582,#2583,#2584,#2585));
#842=EDGE_LOOP('',(#2586));
#843=EDGE_LOOP('',(#2587));
#844=EDGE_LOOP('',(#2588,#2589,#2590,#2591));
#845=EDGE_LOOP('',(#2592));
#846=EDGE_LOOP('',(#2593));
#847=EDGE_LOOP('',(#2594,#2595,#2596,#2597));
#848=EDGE_LOOP('',(#2598));
#849=EDGE_LOOP('',(#2599));
#850=EDGE_LOOP('',(#2600,#2601,#2602,#2603));
#851=EDGE_LOOP('',(#2604,#2605,#2606,#2607));
#852=EDGE_LOOP('',(#2608,#2609,#2610,#2611));
#853=EDGE_LOOP('',(#2612));
#854=EDGE_LOOP('',(#2613));
#855=EDGE_LOOP('',(#2614));
#856=EDGE_LOOP('',(#2615));
#857=EDGE_LOOP('',(#2616,#2617,#2618,#2619));
#858=EDGE_LOOP('',(#2620,#2621,#2622,#2623));
#859=EDGE_LOOP('',(#2624,#2625,#2626,#2627));
#860=EDGE_LOOP('',(#2628,#2629,#2630,#2631));
#861=EDGE_LOOP('',(#2632,#2633,#2634,#2635,#2636,#2637,#2638,#2639,#2640));
#862=EDGE_LOOP('',(#2641));
#863=EDGE_LOOP('',(#2642,#2643,#2644,#2645));
#864=EDGE_LOOP('',(#2646,#2647,#2648,#2649));
#865=EDGE_LOOP('',(#2650,#2651,#2652,#2653));
#866=EDGE_LOOP('',(#2654,#2655,#2656,#2657));
#867=EDGE_LOOP('',(#2658,#2659,#2660,#2661));
#868=EDGE_LOOP('',(#2662,#2663,#2664,#2665,#2666,#2667,#2668,#2669,#2670));
#869=EDGE_LOOP('',(#2671));
#870=EDGE_LOOP('',(#2672,#2673,#2674,#2675));
#871=EDGE_LOOP('',(#2676,#2677,#2678,#2679));
#872=EDGE_LOOP('',(#2680,#2681,#2682,#2683));
#873=EDGE_LOOP('',(#2684,#2685,#2686,#2687));
#874=EDGE_LOOP('',(#2688,#2689,#2690,#2691));
#875=EDGE_LOOP('',(#2692,#2693,#2694,#2695));
#876=EDGE_LOOP('',(#2696,#2697,#2698,#2699));
#877=LINE('',#4501,#1089);
#878=LINE('',#4503,#1090);
#879=LINE('',#4505,#1091);
#880=LINE('',#4506,#1092);
#881=LINE('',#4509,#1093);
#882=LINE('',#4511,#1094);
#883=LINE('',#4513,#1095);
#884=LINE('',#4515,#1096);
#885=LINE('',#4517,#1097);
#886=LINE('',#4519,#1098);
#887=LINE('',#4520,#1099);
#888=LINE('',#4523,#1100);
#889=LINE('',#4525,#1101);
#890=LINE('',#4526,#1102);
#891=LINE('',#4530,#1103);
#892=LINE('',#4532,#1104);
#893=LINE('',#4534,#1105);
#894=LINE('',#4535,#1106);
#895=LINE('',#4538,#1107);
#896=LINE('',#4540,#1108);
#897=LINE('',#4541,#1109);
#898=LINE('',#4543,#1110);
#899=LINE('',#4545,#1111);
#900=LINE('',#4546,#1112);
#901=LINE('',#4548,#1113);
#902=LINE('',#4549,#1114);
#903=LINE('',#4552,#1115);
#904=LINE('',#4554,#1116);
#905=LINE('',#4555,#1117);
#906=LINE('',#4560,#1118);
#907=LINE('',#4562,#1119);
#908=LINE('',#4563,#1120);
#909=LINE('',#4566,#1121);
#910=LINE('',#4568,#1122);
#911=LINE('',#4570,#1123);
#912=LINE('',#4571,#1124);
#913=LINE('',#4576,#1125);
#914=LINE('',#4580,#1126);
#915=LINE('',#4584,#1127);
#916=LINE('',#4586,#1128);
#917=LINE('',#4587,#1129);
#918=LINE('',#4589,#1130);
#919=LINE('',#4590,#1131);
#920=LINE('',#4594,#1132);
#921=LINE('',#4595,#1133);
#922=LINE('',#4598,#1134);
#923=LINE('',#4600,#1135);
#924=LINE('',#4601,#1136);
#925=LINE('',#4603,#1137);
#926=LINE('',#4605,#1138);
#927=LINE('',#4611,#1139);
#928=LINE('',#4614,#1140);
#929=LINE('',#4620,#1141);
#930=LINE('',#4623,#1142);
#931=LINE('',#4626,#1143);
#932=LINE('',#4628,#1144);
#933=LINE('',#4630,#1145);
#934=LINE('',#4632,#1146);
#935=LINE('',#4633,#1147);
#936=LINE('',#4636,#1148);
#937=LINE('',#4637,#1149);
#938=LINE('',#4640,#1150);
#939=LINE('',#4642,#1151);
#940=LINE('',#4644,#1152);
#941=LINE('',#4646,#1153);
#942=LINE('',#4647,#1154);
#943=LINE('',#4650,#1155);
#944=LINE('',#4651,#1156);
#945=LINE('',#4654,#1157);
#946=LINE('',#4656,#1158);
#947=LINE('',#4658,#1159);
#948=LINE('',#4659,#1160);
#949=LINE('',#4661,#1161);
#950=LINE('',#4663,#1162);
#951=LINE('',#4664,#1163);
#952=LINE('',#4668,#1164);
#953=LINE('',#4670,#1165);
#954=LINE('',#4672,#1166);
#955=LINE('',#4673,#1167);
#956=LINE('',#4675,#1168);
#957=LINE('',#4677,#1169);
#958=LINE('',#4678,#1170);
#959=LINE('',#4684,#1171);
#960=LINE('',#4690,#1172);
#961=LINE('',#4696,#1173);
#962=LINE('',#4702,#1174);
#963=LINE('',#4707,#1175);
#964=LINE('',#4709,#1176);
#965=LINE('',#4711,#1177);
#966=LINE('',#4712,#1178);
#967=LINE('',#4715,#1179);
#968=LINE('',#4717,#1180);
#969=LINE('',#4718,#1181);
#970=LINE('',#4721,#1182);
#971=LINE('',#4723,#1183);
#972=LINE('',#4724,#1184);
#973=LINE('',#4726,#1185);
#974=LINE('',#4727,#1186);
#975=LINE('',#4735,#1187);
#976=LINE('',#4745,#1188);
#977=LINE('',#4751,#1189);
#978=LINE('',#4758,#1190);
#979=LINE('',#4764,#1191);
#980=LINE('',#4773,#1192);
#981=LINE('',#4779,#1193);
#982=LINE('',#4787,#1194);
#983=LINE('',#4789,#1195);
#984=LINE('',#4791,#1196);
#985=LINE('',#4792,#1197);
#986=LINE('',#4795,#1198);
#987=LINE('',#4797,#1199);
#988=LINE('',#4798,#1200);
#989=LINE('',#4801,#1201);
#990=LINE('',#4803,#1202);
#991=LINE('',#4804,#1203);
#992=LINE('',#4807,#1204);
#993=LINE('',#4809,#1205);
#994=LINE('',#4810,#1206);
#995=LINE('',#4813,#1207);
#996=LINE('',#4815,#1208);
#997=LINE('',#4816,#1209);
#998=LINE('',#4818,#1210);
#999=LINE('',#4819,#1211);
#1000=LINE('',#4831,#1212);
#1001=LINE('',#4835,#1213);
#1002=LINE('',#4839,#1214);
#1003=LINE('',#4846,#1215);
#1004=LINE('',#4848,#1216);
#1005=LINE('',#4854,#1217);
#1006=LINE('',#4860,#1218);
#1007=LINE('',#4869,#1219);
#1008=LINE('',#4874,#1220);
#1009=LINE('',#4880,#1221);
#1010=LINE('',#4906,#1222);
#1011=LINE('',#4908,#1223);
#1012=LINE('',#4909,#1224);
#1013=LINE('',#4912,#1225);
#1014=LINE('',#4913,#1226);
#1015=LINE('',#4916,#1227);
#1016=LINE('',#4917,#1228);
#1017=LINE('',#4920,#1229);
#1018=LINE('',#4921,#1230);
#1019=LINE('',#4924,#1231);
#1020=LINE('',#4925,#1232);
#1021=LINE('',#4927,#1233);
#1022=LINE('',#4942,#1234);
#1023=LINE('',#4963,#1235);
#1024=LINE('',#4988,#1236);
#1025=LINE('',#4989,#1237);
#1026=LINE('',#4991,#1238);
#1027=LINE('',#4993,#1239);
#1028=LINE('',#4998,#1240);
#1029=LINE('',#5001,#1241);
#1030=LINE('',#5003,#1242);
#1031=LINE('',#5023,#1243);
#1032=LINE('',#5032,#1244);
#1033=LINE('',#5038,#1245);
#1034=LINE('',#5043,#1246);
#1035=LINE('',#5061,#1247);
#1036=LINE('',#5067,#1248);
#1037=LINE('',#5071,#1249);
#1038=LINE('',#5077,#1250);
#1039=LINE('',#5082,#1251);
#1040=LINE('',#5097,#1252);
#1041=LINE('',#5106,#1253);
#1042=LINE('',#5110,#1254);
#1043=LINE('',#5114,#1255);
#1044=LINE('',#5117,#1256);
#1045=LINE('',#5253,#1257);
#1046=LINE('',#5506,#1258);
#1047=LINE('',#5548,#1259);
#1048=LINE('',#5553,#1260);
#1049=LINE('',#5562,#1261);
#1050=LINE('',#5567,#1262);
#1051=LINE('',#5578,#1263);
#1052=LINE('',#5584,#1264);
#1053=LINE('',#5599,#1265);
#1054=LINE('',#5604,#1266);
#1055=LINE('',#5606,#1267);
#1056=LINE('',#5608,#1268);
#1057=LINE('',#5609,#1269);
#1058=LINE('',#5612,#1270);
#1059=LINE('',#5614,#1271);
#1060=LINE('',#5615,#1272);
#1061=LINE('',#5619,#1273);
#1062=LINE('',#5620,#1274);
#1063=LINE('',#5621,#1275);
#1064=LINE('',#5626,#1276);
#1065=LINE('',#5628,#1277);
#1066=LINE('',#5630,#1278);
#1067=LINE('',#5632,#1279);
#1068=LINE('',#5637,#1280);
#1069=LINE('',#5640,#1281);
#1070=LINE('',#5642,#1282);
#1071=LINE('',#5643,#1283);
#1072=LINE('',#5646,#1284);
#1073=LINE('',#5647,#1285);
#1074=LINE('',#5650,#1286);
#1075=LINE('',#5651,#1287);
#1076=LINE('',#5653,#1288);
#1077=LINE('',#5661,#1289);
#1078=LINE('',#5663,#1290);
#1079=LINE('',#5665,#1291);
#1080=LINE('',#5666,#1292);
#1081=LINE('',#5669,#1293);
#1082=LINE('',#5671,#1294);
#1083=LINE('',#5672,#1295);
#1084=LINE('',#5675,#1296);
#1085=LINE('',#5677,#1297);
#1086=LINE('',#5678,#1298);
#1087=LINE('',#5680,#1299);
#1088=LINE('',#5681,#1300);
#1089=VECTOR('',#3569,1.);
#1090=VECTOR('',#3570,1.);
#1091=VECTOR('',#3571,1.);
#1092=VECTOR('',#3572,1.);
#1093=VECTOR('',#3575,1.);
#1094=VECTOR('',#3576,1.);
#1095=VECTOR('',#3577,1.);
#1096=VECTOR('',#3578,1.);
#1097=VECTOR('',#3579,1.);
#1098=VECTOR('',#3580,1.);
#1099=VECTOR('',#3581,1.);
#1100=VECTOR('',#3584,1.);
#1101=VECTOR('',#3585,1.);
#1102=VECTOR('',#3586,1.);
#1103=VECTOR('',#3589,1.);
#1104=VECTOR('',#3590,1.);
#1105=VECTOR('',#3591,1.);
#1106=VECTOR('',#3592,1.);
#1107=VECTOR('',#3595,1.);
#1108=VECTOR('',#3596,1.);
#1109=VECTOR('',#3597,1.);
#1110=VECTOR('',#3598,1.);
#1111=VECTOR('',#3599,1.);
#1112=VECTOR('',#3600,1.);
#1113=VECTOR('',#3603,1.);
#1114=VECTOR('',#3604,1.);
#1115=VECTOR('',#3607,1.);
#1116=VECTOR('',#3608,1.);
#1117=VECTOR('',#3609,1.);
#1118=VECTOR('',#3614,1.);
#1119=VECTOR('',#3615,1.);
#1120=VECTOR('',#3616,1.);
#1121=VECTOR('',#3619,1.);
#1122=VECTOR('',#3620,1.);
#1123=VECTOR('',#3621,1.);
#1124=VECTOR('',#3622,1.);
#1125=VECTOR('',#3627,0.325);
#1126=VECTOR('',#3632,0.325);
#1127=VECTOR('',#3637,1.);
#1128=VECTOR('',#3638,1.);
#1129=VECTOR('',#3639,1.);
#1130=VECTOR('',#3642,1.);
#1131=VECTOR('',#3643,1.);
#1132=VECTOR('',#3648,1.);
#1133=VECTOR('',#3649,1.);
#1134=VECTOR('',#3652,1.);
#1135=VECTOR('',#3653,1.);
#1136=VECTOR('',#3654,1.);
#1137=VECTOR('',#3657,1.);
#1138=VECTOR('',#3660,1.);
#1139=VECTOR('',#3665,1.);
#1140=VECTOR('',#3668,1.);
#1141=VECTOR('',#3673,1.);
#1142=VECTOR('',#3676,1.);
#1143=VECTOR('',#3679,1.);
#1144=VECTOR('',#3680,1.);
#1145=VECTOR('',#3681,1.);
#1146=VECTOR('',#3682,1.);
#1147=VECTOR('',#3683,1.);
#1148=VECTOR('',#3686,1.);
#1149=VECTOR('',#3687,1.);
#1150=VECTOR('',#3690,1.);
#1151=VECTOR('',#3691,1.);
#1152=VECTOR('',#3692,1.);
#1153=VECTOR('',#3693,1.);
#1154=VECTOR('',#3694,1.);
#1155=VECTOR('',#3697,1.);
#1156=VECTOR('',#3698,1.);
#1157=VECTOR('',#3701,1.);
#1158=VECTOR('',#3702,1.);
#1159=VECTOR('',#3703,1.);
#1160=VECTOR('',#3704,1.);
#1161=VECTOR('',#3707,1.);
#1162=VECTOR('',#3710,1.);
#1163=VECTOR('',#3711,1.);
#1164=VECTOR('',#3716,1.);
#1165=VECTOR('',#3717,1.);
#1166=VECTOR('',#3718,1.);
#1167=VECTOR('',#3719,1.);
#1168=VECTOR('',#3722,1.);
#1169=VECTOR('',#3725,1.);
#1170=VECTOR('',#3726,1.);
#1171=VECTOR('',#3733,0.425);
#1172=VECTOR('',#3740,0.425);
#1173=VECTOR('',#3747,0.425);
#1174=VECTOR('',#3754,0.425);
#1175=VECTOR('',#3759,1.);
#1176=VECTOR('',#3760,1.);
#1177=VECTOR('',#3761,1.);
#1178=VECTOR('',#3762,1.);
#1179=VECTOR('',#3765,1.);
#1180=VECTOR('',#3766,1.);
#1181=VECTOR('',#3767,1.);
#1182=VECTOR('',#3770,1.);
#1183=VECTOR('',#3771,1.);
#1184=VECTOR('',#3772,1.);
#1185=VECTOR('',#3775,1.);
#1186=VECTOR('',#3776,1.);
#1187=VECTOR('',#3787,0.165);
#1188=VECTOR('',#3800,0.9);
#1189=VECTOR('',#3809,0.6);
#1190=VECTOR('',#3818,0.605);
#1191=VECTOR('',#3825,0.8);
#1192=VECTOR('',#3838,0.225);
#1193=VECTOR('',#3845,0.8);
#1194=VECTOR('',#3856,1.);
#1195=VECTOR('',#3857,1.);
#1196=VECTOR('',#3858,1.);
#1197=VECTOR('',#3859,1.);
#1198=VECTOR('',#3862,1.);
#1199=VECTOR('',#3863,1.);
#1200=VECTOR('',#3864,1.);
#1201=VECTOR('',#3867,1.);
#1202=VECTOR('',#3868,1.);
#1203=VECTOR('',#3869,1.);
#1204=VECTOR('',#3872,1.);
#1205=VECTOR('',#3873,1.);
#1206=VECTOR('',#3874,1.);
#1207=VECTOR('',#3877,1.);
#1208=VECTOR('',#3878,1.);
#1209=VECTOR('',#3879,1.);
#1210=VECTOR('',#3882,1.);
#1211=VECTOR('',#3883,1.);
#1212=VECTOR('',#3900,0.325);
#1213=VECTOR('',#3905,0.35);
#1214=VECTOR('',#3910,0.335);
#1215=VECTOR('',#3919,0.21);
#1216=VECTOR('',#3922,0.2);
#1217=VECTOR('',#3929,0.32);
#1218=VECTOR('',#3936,0.6);
#1219=VECTOR('',#3949,0.3);
#1220=VECTOR('',#3956,0.27);
#1221=VECTOR('',#3963,0.576175134594813);
#1222=VECTOR('',#3966,1.);
#1223=VECTOR('',#3967,1.);
#1224=VECTOR('',#3968,1.);
#1225=VECTOR('',#3971,1.);
#1226=VECTOR('',#3972,1.);
#1227=VECTOR('',#3975,1.);
#1228=VECTOR('',#3976,1.);
#1229=VECTOR('',#3979,1.);
#1230=VECTOR('',#3980,1.);
#1231=VECTOR('',#3983,1.);
#1232=VECTOR('',#3984,1.);
#1233=VECTOR('',#3987,1.);
#1234=VECTOR('',#3996,0.576175134594813);
#1235=VECTOR('',#4003,0.576175134594813);
#1236=VECTOR('',#4006,1.);
#1237=VECTOR('',#4007,1.);
#1238=VECTOR('',#4010,1.);
#1239=VECTOR('',#4013,1.);
#1240=VECTOR('',#4018,0.3);
#1241=VECTOR('',#4023,1.);
#1242=VECTOR('',#4026,1.);
#1243=VECTOR('',#4061,1.6);
#1244=VECTOR('',#4072,1.6);
#1245=VECTOR('',#4081,0.62);
#1246=VECTOR('',#4086,3.75);
#1247=VECTOR('',#4111,1.070235);
#1248=VECTOR('',#4118,0.6);
#1249=VECTOR('',#4123,0.63);
#1250=VECTOR('',#4132,1.070235);
#1251=VECTOR('',#4139,0.63);
#1252=VECTOR('',#4158,1.129765);
#1253=VECTOR('',#4169,1.57);
#1254=VECTOR('',#4174,1.6);
#1255=VECTOR('',#4179,1.57);
#1256=VECTOR('',#4184,1.129765);
#1257=VECTOR('',#4231,1.123812);
#1258=VECTOR('',#4300,1.076188);
#1259=VECTOR('',#4329,1.119765);
#1260=VECTOR('',#4336,1.085235);
#1261=VECTOR('',#4347,1.119765);
#1262=VECTOR('',#4354,1.085235);
#1263=VECTOR('',#4371,1.2);
#1264=VECTOR('',#4378,1.6);
#1265=VECTOR('',#4403,0.325);
#1266=VECTOR('',#4408,1.);
#1267=VECTOR('',#4409,1.);
#1268=VECTOR('',#4410,1.);
#1269=VECTOR('',#4411,1.);
#1270=VECTOR('',#4414,1.);
#1271=VECTOR('',#4415,1.);
#1272=VECTOR('',#4416,1.);
#1273=VECTOR('',#4419,1.);
#1274=VECTOR('',#4420,1.);
#1275=VECTOR('',#4421,1.);
#1276=VECTOR('',#4426,1.);
#1277=VECTOR('',#4427,1.);
#1278=VECTOR('',#4428,1.);
#1279=VECTOR('',#4429,1.);
#1280=VECTOR('',#4436,1.);
#1281=VECTOR('',#4439,1.);
#1282=VECTOR('',#4440,1.);
#1283=VECTOR('',#4441,1.);
#1284=VECTOR('',#4444,1.);
#1285=VECTOR('',#4445,1.);
#1286=VECTOR('',#4448,1.);
#1287=VECTOR('',#4449,1.);
#1288=VECTOR('',#4452,1.);
#1289=VECTOR('',#4463,1.);
#1290=VECTOR('',#4464,1.);
#1291=VECTOR('',#4465,1.);
#1292=VECTOR('',#4466,1.);
#1293=VECTOR('',#4469,1.);
#1294=VECTOR('',#4470,1.);
#1295=VECTOR('',#4471,1.);
#1296=VECTOR('',#4474,1.);
#1297=VECTOR('',#4475,1.);
#1298=VECTOR('',#4476,1.);
#1299=VECTOR('',#4479,1.);
#1300=VECTOR('',#4480,1.);
#1301=VERTEX_POINT('',#4499);
#1302=VERTEX_POINT('',#4500);
#1303=VERTEX_POINT('',#4502);
#1304=VERTEX_POINT('',#4504);
#1305=VERTEX_POINT('',#4508);
#1306=VERTEX_POINT('',#4510);
#1307=VERTEX_POINT('',#4512);
#1308=VERTEX_POINT('',#4514);
#1309=VERTEX_POINT('',#4516);
#1310=VERTEX_POINT('',#4518);
#1311=VERTEX_POINT('',#4522);
#1312=VERTEX_POINT('',#4524);
#1313=VERTEX_POINT('',#4528);
#1314=VERTEX_POINT('',#4529);
#1315=VERTEX_POINT('',#4531);
#1316=VERTEX_POINT('',#4533);
#1317=VERTEX_POINT('',#4537);
#1318=VERTEX_POINT('',#4539);
#1319=VERTEX_POINT('',#4542);
#1320=VERTEX_POINT('',#4544);
#1321=VERTEX_POINT('',#4551);
#1322=VERTEX_POINT('',#4553);
#1323=VERTEX_POINT('',#4556);
#1324=VERTEX_POINT('',#4559);
#1325=VERTEX_POINT('',#4561);
#1326=VERTEX_POINT('',#4565);
#1327=VERTEX_POINT('',#4567);
#1328=VERTEX_POINT('',#4569);
#1329=VERTEX_POINT('',#4573);
#1330=VERTEX_POINT('',#4575);
#1331=VERTEX_POINT('',#4579);
#1332=VERTEX_POINT('',#4583);
#1333=VERTEX_POINT('',#4585);
#1334=VERTEX_POINT('',#4593);
#1335=VERTEX_POINT('',#4597);
#1336=VERTEX_POINT('',#4599);
#1337=VERTEX_POINT('',#4607);
#1338=VERTEX_POINT('',#4608);
#1339=VERTEX_POINT('',#4610);
#1340=VERTEX_POINT('',#4612);
#1341=VERTEX_POINT('',#4616);
#1342=VERTEX_POINT('',#4617);
#1343=VERTEX_POINT('',#4619);
#1344=VERTEX_POINT('',#4621);
#1345=VERTEX_POINT('',#4625);
#1346=VERTEX_POINT('',#4627);
#1347=VERTEX_POINT('',#4629);
#1348=VERTEX_POINT('',#4631);
#1349=VERTEX_POINT('',#4635);
#1350=VERTEX_POINT('',#4639);
#1351=VERTEX_POINT('',#4641);
#1352=VERTEX_POINT('',#4643);
#1353=VERTEX_POINT('',#4645);
#1354=VERTEX_POINT('',#4649);
#1355=VERTEX_POINT('',#4653);
#1356=VERTEX_POINT('',#4655);
#1357=VERTEX_POINT('',#4657);
#1358=VERTEX_POINT('',#4667);
#1359=VERTEX_POINT('',#4669);
#1360=VERTEX_POINT('',#4671);
#1361=VERTEX_POINT('',#4681);
#1362=VERTEX_POINT('',#4683);
#1363=VERTEX_POINT('',#4687);
#1364=VERTEX_POINT('',#4689);
#1365=VERTEX_POINT('',#4693);
#1366=VERTEX_POINT('',#4695);
#1367=VERTEX_POINT('',#4699);
#1368=VERTEX_POINT('',#4701);
#1369=VERTEX_POINT('',#4705);
#1370=VERTEX_POINT('',#4706);
#1371=VERTEX_POINT('',#4708);
#1372=VERTEX_POINT('',#4710);
#1373=VERTEX_POINT('',#4714);
#1374=VERTEX_POINT('',#4716);
#1375=VERTEX_POINT('',#4720);
#1376=VERTEX_POINT('',#4722);
#1377=VERTEX_POINT('',#4732);
#1378=VERTEX_POINT('',#4734);
#1379=VERTEX_POINT('',#4739);
#1380=VERTEX_POINT('',#4741);
#1381=VERTEX_POINT('',#4744);
#1382=VERTEX_POINT('',#4749);
#1383=VERTEX_POINT('',#4755);
#1384=VERTEX_POINT('',#4757);
#1385=VERTEX_POINT('',#4761);
#1386=VERTEX_POINT('',#4763);
#1387=VERTEX_POINT('',#4770);
#1388=VERTEX_POINT('',#4772);
#1389=VERTEX_POINT('',#4776);
#1390=VERTEX_POINT('',#4778);
#1391=VERTEX_POINT('',#4785);
#1392=VERTEX_POINT('',#4786);
#1393=VERTEX_POINT('',#4788);
#1394=VERTEX_POINT('',#4790);
#1395=VERTEX_POINT('',#4794);
#1396=VERTEX_POINT('',#4796);
#1397=VERTEX_POINT('',#4800);
#1398=VERTEX_POINT('',#4802);
#1399=VERTEX_POINT('',#4806);
#1400=VERTEX_POINT('',#4808);
#1401=VERTEX_POINT('',#4812);
#1402=VERTEX_POINT('',#4814);
#1403=VERTEX_POINT('',#4823);
#1404=VERTEX_POINT('',#4826);
#1405=VERTEX_POINT('',#4829);
#1406=VERTEX_POINT('',#4833);
#1407=VERTEX_POINT('',#4837);
#1408=VERTEX_POINT('',#4841);
#1409=VERTEX_POINT('',#4844);
#1410=VERTEX_POINT('',#4851);
#1411=VERTEX_POINT('',#4853);
#1412=VERTEX_POINT('',#4857);
#1413=VERTEX_POINT('',#4859);
#1414=VERTEX_POINT('',#4866);
#1415=VERTEX_POINT('',#4868);
#1416=VERTEX_POINT('',#4872);
#1417=VERTEX_POINT('',#4877);
#1418=VERTEX_POINT('',#4879);
#1419=VERTEX_POINT('',#4881);
#1420=VERTEX_POINT('',#4885);
#1421=VERTEX_POINT('',#4889);
#1422=VERTEX_POINT('',#4893);
#1423=VERTEX_POINT('',#4897);
#1424=VERTEX_POINT('',#4905);
#1425=VERTEX_POINT('',#4907);
#1426=VERTEX_POINT('',#4911);
#1427=VERTEX_POINT('',#4915);
#1428=VERTEX_POINT('',#4919);
#1429=VERTEX_POINT('',#4923);
#1430=VERTEX_POINT('',#4932);
#1431=VERTEX_POINT('',#4933);
#1432=VERTEX_POINT('',#4937);
#1433=VERTEX_POINT('',#4941);
#1434=VERTEX_POINT('',#4944);
#1435=VERTEX_POINT('',#4948);
#1436=VERTEX_POINT('',#4952);
#1437=VERTEX_POINT('',#4960);
#1438=VERTEX_POINT('',#4962);
#1439=VERTEX_POINT('',#4964);
#1440=VERTEX_POINT('',#4968);
#1441=VERTEX_POINT('',#4972);
#1442=VERTEX_POINT('',#4976);
#1443=VERTEX_POINT('',#4980);
#1444=VERTEX_POINT('',#4995);
#1445=VERTEX_POINT('',#4997);
#1446=VERTEX_POINT('',#5020);
#1447=VERTEX_POINT('',#5022);
#1448=VERTEX_POINT('',#5026);
#1449=VERTEX_POINT('',#5029);
#1450=VERTEX_POINT('',#5031);
#1451=VERTEX_POINT('',#5035);
#1452=VERTEX_POINT('',#5040);
#1453=VERTEX_POINT('',#5042);
#1454=VERTEX_POINT('',#5050);
#1455=VERTEX_POINT('',#5051);
#1456=VERTEX_POINT('',#5054);
#1457=VERTEX_POINT('',#5056);
#1458=VERTEX_POINT('',#5060);
#1459=VERTEX_POINT('',#5064);
#1460=VERTEX_POINT('',#5066);
#1461=VERTEX_POINT('',#5070);
#1462=VERTEX_POINT('',#5075);
#1463=VERTEX_POINT('',#5079);
#1464=VERTEX_POINT('',#5085);
#1465=VERTEX_POINT('',#5086);
#1466=VERTEX_POINT('',#5089);
#1467=VERTEX_POINT('',#5091);
#1468=VERTEX_POINT('',#5095);
#1469=VERTEX_POINT('',#5099);
#1470=VERTEX_POINT('',#5101);
#1471=VERTEX_POINT('',#5104);
#1472=VERTEX_POINT('',#5108);
#1473=VERTEX_POINT('',#5112);
#1474=VERTEX_POINT('',#5120);
#1475=VERTEX_POINT('',#5121);
#1476=VERTEX_POINT('',#5124);
#1477=VERTEX_POINT('',#5125);
#1478=VERTEX_POINT('',#5128);
#1479=VERTEX_POINT('',#5129);
#1480=VERTEX_POINT('',#5132);
#1481=VERTEX_POINT('',#5133);
#1482=VERTEX_POINT('',#5136);
#1483=VERTEX_POINT('',#5137);
#1484=VERTEX_POINT('',#5140);
#1485=VERTEX_POINT('',#5141);
#1486=VERTEX_POINT('',#5144);
#1487=VERTEX_POINT('',#5145);
#1488=VERTEX_POINT('',#5149);
#1489=VERTEX_POINT('',#5150);
#1490=VERTEX_POINT('',#5173);
#1491=VERTEX_POINT('',#5175);
#1492=VERTEX_POINT('',#5200);
#1493=VERTEX_POINT('',#5202);
#1494=VERTEX_POINT('',#5225);
#1495=VERTEX_POINT('',#5227);
#1496=VERTEX_POINT('',#5250);
#1497=VERTEX_POINT('',#5252);
#1498=VERTEX_POINT('',#5255);
#1499=VERTEX_POINT('',#5257);
#1500=VERTEX_POINT('',#5280);
#1501=VERTEX_POINT('',#5282);
#1502=VERTEX_POINT('',#5305);
#1503=VERTEX_POINT('',#5307);
#1504=VERTEX_POINT('',#5330);
#1505=VERTEX_POINT('',#5332);
#1506=VERTEX_POINT('',#5357);
#1507=VERTEX_POINT('',#5361);
#1508=VERTEX_POINT('',#5386);
#1509=VERTEX_POINT('',#5390);
#1510=VERTEX_POINT('',#5415);
#1511=VERTEX_POINT('',#5417);
#1512=VERTEX_POINT('',#5421);
#1513=VERTEX_POINT('',#5446);
#1514=VERTEX_POINT('',#5450);
#1515=VERTEX_POINT('',#5475);
#1516=VERTEX_POINT('',#5479);
#1517=VERTEX_POINT('',#5504);
#1518=VERTEX_POINT('',#5507);
#1519=VERTEX_POINT('',#5509);
#1520=VERTEX_POINT('',#5541);
#1521=VERTEX_POINT('',#5543);
#1522=VERTEX_POINT('',#5546);
#1523=VERTEX_POINT('',#5550);
#1524=VERTEX_POINT('',#5555);
#1525=VERTEX_POINT('',#5557);
#1526=VERTEX_POINT('',#5560);
#1527=VERTEX_POINT('',#5564);
#1528=VERTEX_POINT('',#5575);
#1529=VERTEX_POINT('',#5577);
#1530=VERTEX_POINT('',#5581);
#1531=VERTEX_POINT('',#5583);
#1532=VERTEX_POINT('',#5596);
#1533=VERTEX_POINT('',#5598);
#1534=VERTEX_POINT('',#5602);
#1535=VERTEX_POINT('',#5603);
#1536=VERTEX_POINT('',#5605);
#1537=VERTEX_POINT('',#5607);
#1538=VERTEX_POINT('',#5611);
#1539=VERTEX_POINT('',#5613);
#1540=VERTEX_POINT('',#5617);
#1541=VERTEX_POINT('',#5618);
#1542=VERTEX_POINT('',#5623);
#1543=VERTEX_POINT('',#5625);
#1544=VERTEX_POINT('',#5627);
#1545=VERTEX_POINT('',#5629);
#1546=VERTEX_POINT('',#5631);
#1547=VERTEX_POINT('',#5635);
#1548=VERTEX_POINT('',#5639);
#1549=VERTEX_POINT('',#5641);
#1550=VERTEX_POINT('',#5645);
#1551=VERTEX_POINT('',#5649);
#1552=VERTEX_POINT('',#5659);
#1553=VERTEX_POINT('',#5660);
#1554=VERTEX_POINT('',#5662);
#1555=VERTEX_POINT('',#5664);
#1556=VERTEX_POINT('',#5668);
#1557=VERTEX_POINT('',#5670);
#1558=VERTEX_POINT('',#5674);
#1559=VERTEX_POINT('',#5676);
#1560=EDGE_CURVE('',#1301,#1302,#877,.T.);
#1561=EDGE_CURVE('',#1303,#1301,#878,.T.);
#1562=EDGE_CURVE('',#1304,#1303,#879,.T.);
#1563=EDGE_CURVE('',#1304,#1302,#880,.T.);
#1564=EDGE_CURVE('',#1305,#1301,#881,.T.);
#1565=EDGE_CURVE('',#1306,#1305,#882,.T.);
#1566=EDGE_CURVE('',#1307,#1306,#883,.T.);
#1567=EDGE_CURVE('',#1308,#1307,#884,.T.);
#1568=EDGE_CURVE('',#1309,#1308,#885,.T.);
#1569=EDGE_CURVE('',#1310,#1309,#886,.T.);
#1570=EDGE_CURVE('',#1303,#1310,#887,.T.);
#1571=EDGE_CURVE('',#1311,#1308,#888,.T.);
#1572=EDGE_CURVE('',#1312,#1311,#889,.T.);
#1573=EDGE_CURVE('',#1309,#1312,#890,.T.);
#1574=EDGE_CURVE('',#1313,#1314,#891,.T.);
#1575=EDGE_CURVE('',#1313,#1315,#892,.T.);
#1576=EDGE_CURVE('',#1316,#1315,#893,.T.);
#1577=EDGE_CURVE('',#1314,#1316,#894,.T.);
#1578=EDGE_CURVE('',#1302,#1317,#895,.T.);
#1579=EDGE_CURVE('',#1318,#1304,#896,.T.);
#1580=EDGE_CURVE('',#1315,#1318,#897,.T.);
#1581=EDGE_CURVE('',#1319,#1313,#898,.T.);
#1582=EDGE_CURVE('',#1320,#1319,#899,.T.);
#1583=EDGE_CURVE('',#1320,#1317,#900,.T.);
#1584=EDGE_CURVE('',#1317,#1305,#901,.T.);
#1585=EDGE_CURVE('',#1306,#1320,#902,.T.);
#1586=EDGE_CURVE('',#1316,#1321,#903,.T.);
#1587=EDGE_CURVE('',#1321,#1322,#904,.T.);
#1588=EDGE_CURVE('',#1322,#1314,#905,.T.);
#1589=EDGE_CURVE('',#1323,#1323,#340,.T.);
#1590=EDGE_CURVE('',#1324,#1318,#906,.T.);
#1591=EDGE_CURVE('',#1325,#1324,#907,.T.);
#1592=EDGE_CURVE('',#1321,#1325,#908,.T.);
#1593=EDGE_CURVE('',#1326,#1312,#909,.T.);
#1594=EDGE_CURVE('',#1327,#1326,#910,.T.);
#1595=EDGE_CURVE('',#1328,#1327,#911,.T.);
#1596=EDGE_CURVE('',#1310,#1328,#912,.T.);
#1597=EDGE_CURVE('',#1329,#1329,#341,.T.);
#1598=EDGE_CURVE('',#1329,#1330,#913,.T.);
#1599=EDGE_CURVE('',#1330,#1330,#342,.T.);
#1600=EDGE_CURVE('',#1323,#1331,#914,.T.);
#1601=EDGE_CURVE('',#1331,#1331,#343,.T.);
#1602=EDGE_CURVE('',#1332,#1324,#915,.T.);
#1603=EDGE_CURVE('',#1332,#1333,#916,.T.);
#1604=EDGE_CURVE('',#1333,#1325,#917,.T.);
#1605=EDGE_CURVE('',#1322,#1333,#918,.T.);
#1606=EDGE_CURVE('',#1319,#1332,#919,.T.);
#1607=EDGE_CURVE('',#1311,#1334,#920,.T.);
#1608=EDGE_CURVE('',#1334,#1326,#921,.T.);
#1609=EDGE_CURVE('',#1335,#1307,#922,.T.);
#1610=EDGE_CURVE('',#1336,#1335,#923,.T.);
#1611=EDGE_CURVE('',#1336,#1334,#924,.T.);
#1612=EDGE_CURVE('',#1327,#1336,#925,.T.);
#1613=EDGE_CURVE('',#1328,#1335,#926,.T.);
#1614=EDGE_CURVE('',#1337,#1338,#344,.T.);
#1615=EDGE_CURVE('',#1339,#1337,#927,.T.);
#1616=EDGE_CURVE('',#1340,#1339,#345,.T.);
#1617=EDGE_CURVE('',#1338,#1340,#928,.T.);
#1618=EDGE_CURVE('',#1341,#1342,#346,.T.);
#1619=EDGE_CURVE('',#1343,#1341,#929,.T.);
#1620=EDGE_CURVE('',#1344,#1343,#347,.T.);
#1621=EDGE_CURVE('',#1342,#1344,#930,.T.);
#1622=EDGE_CURVE('',#1343,#1345,#931,.T.);
#1623=EDGE_CURVE('',#1345,#1346,#932,.T.);
#1624=EDGE_CURVE('',#1347,#1346,#933,.T.);
#1625=EDGE_CURVE('',#1347,#1348,#934,.T.);
#1626=EDGE_CURVE('',#1348,#1344,#935,.T.);
#1627=EDGE_CURVE('',#1349,#1341,#936,.T.);
#1628=EDGE_CURVE('',#1345,#1349,#937,.T.);
#1629=EDGE_CURVE('',#1339,#1350,#938,.T.);
#1630=EDGE_CURVE('',#1350,#1351,#939,.T.);
#1631=EDGE_CURVE('',#1352,#1351,#940,.T.);
#1632=EDGE_CURVE('',#1352,#1353,#941,.T.);
#1633=EDGE_CURVE('',#1353,#1340,#942,.T.);
#1634=EDGE_CURVE('',#1354,#1337,#943,.T.);
#1635=EDGE_CURVE('',#1350,#1354,#944,.T.);
#1636=EDGE_CURVE('',#1342,#1355,#945,.T.);
#1637=EDGE_CURVE('',#1355,#1356,#946,.T.);
#1638=EDGE_CURVE('',#1357,#1356,#947,.T.);
#1639=EDGE_CURVE('',#1357,#1349,#948,.T.);
#1640=EDGE_CURVE('',#1346,#1357,#949,.T.);
#1641=EDGE_CURVE('',#1356,#1347,#950,.T.);
#1642=EDGE_CURVE('',#1348,#1355,#951,.T.);
#1643=EDGE_CURVE('',#1338,#1358,#952,.T.);
#1644=EDGE_CURVE('',#1358,#1359,#953,.T.);
#1645=EDGE_CURVE('',#1360,#1359,#954,.T.);
#1646=EDGE_CURVE('',#1360,#1354,#955,.T.);
#1647=EDGE_CURVE('',#1351,#1360,#956,.T.);
#1648=EDGE_CURVE('',#1359,#1352,#957,.T.);
#1649=EDGE_CURVE('',#1353,#1358,#958,.T.);
#1650=EDGE_CURVE('',#1361,#1361,#348,.T.);
#1651=EDGE_CURVE('',#1361,#1362,#959,.T.);
#1652=EDGE_CURVE('',#1362,#1362,#349,.T.);
#1653=EDGE_CURVE('',#1363,#1363,#350,.T.);
#1654=EDGE_CURVE('',#1363,#1364,#960,.T.);
#1655=EDGE_CURVE('',#1364,#1364,#351,.T.);
#1656=EDGE_CURVE('',#1365,#1365,#352,.T.);
#1657=EDGE_CURVE('',#1365,#1366,#961,.T.);
#1658=EDGE_CURVE('',#1366,#1366,#353,.T.);
#1659=EDGE_CURVE('',#1367,#1367,#354,.T.);
#1660=EDGE_CURVE('',#1367,#1368,#962,.T.);
#1661=EDGE_CURVE('',#1368,#1368,#355,.T.);
#1662=EDGE_CURVE('',#1369,#1370,#963,.T.);
#1663=EDGE_CURVE('',#1370,#1371,#964,.T.);
#1664=EDGE_CURVE('',#1372,#1371,#965,.T.);
#1665=EDGE_CURVE('',#1369,#1372,#966,.T.);
#1666=EDGE_CURVE('',#1373,#1369,#967,.T.);
#1667=EDGE_CURVE('',#1374,#1372,#968,.T.);
#1668=EDGE_CURVE('',#1373,#1374,#969,.T.);
#1669=EDGE_CURVE('',#1375,#1373,#970,.T.);
#1670=EDGE_CURVE('',#1376,#1374,#971,.T.);
#1671=EDGE_CURVE('',#1375,#1376,#972,.T.);
#1672=EDGE_CURVE('',#1370,#1375,#973,.T.);
#1673=EDGE_CURVE('',#1371,#1376,#974,.T.);
#1674=EDGE_CURVE('',#1377,#1377,#356,.T.);
#1675=EDGE_CURVE('',#1377,#1378,#975,.T.);
#1676=EDGE_CURVE('',#1378,#1378,#357,.T.);
#1677=EDGE_CURVE('',#1379,#1379,#358,.T.);
#1678=EDGE_CURVE('',#1380,#1380,#359,.T.);
#1679=EDGE_CURVE('',#1379,#1381,#976,.T.);
#1680=EDGE_CURVE('',#1381,#1381,#360,.T.);
#1681=EDGE_CURVE('',#1382,#1382,#361,.T.);
#1682=EDGE_CURVE('',#1382,#1380,#977,.T.);
#1683=EDGE_CURVE('',#1383,#1383,#362,.T.);
#1684=EDGE_CURVE('',#1383,#1384,#978,.T.);
#1685=EDGE_CURVE('',#1384,#1384,#363,.T.);
#1686=EDGE_CURVE('',#1385,#1385,#364,.T.);
#1687=EDGE_CURVE('',#1385,#1386,#979,.T.);
#1688=EDGE_CURVE('',#1386,#1386,#365,.T.);
#1689=EDGE_CURVE('',#1387,#1387,#366,.T.);
#1690=EDGE_CURVE('',#1387,#1388,#980,.T.);
#1691=EDGE_CURVE('',#1388,#1388,#367,.T.);
#1692=EDGE_CURVE('',#1389,#1389,#368,.T.);
#1693=EDGE_CURVE('',#1389,#1390,#981,.T.);
#1694=EDGE_CURVE('',#1390,#1390,#369,.T.);
#1695=EDGE_CURVE('',#1391,#1392,#982,.T.);
#1696=EDGE_CURVE('',#1392,#1393,#983,.T.);
#1697=EDGE_CURVE('',#1393,#1394,#984,.T.);
#1698=EDGE_CURVE('',#1391,#1394,#985,.T.);
#1699=EDGE_CURVE('',#1392,#1395,#986,.T.);
#1700=EDGE_CURVE('',#1395,#1396,#987,.T.);
#1701=EDGE_CURVE('',#1396,#1393,#988,.T.);
#1702=EDGE_CURVE('',#1395,#1397,#989,.T.);
#1703=EDGE_CURVE('',#1397,#1398,#990,.T.);
#1704=EDGE_CURVE('',#1398,#1396,#991,.T.);
#1705=EDGE_CURVE('',#1397,#1399,#992,.T.);
#1706=EDGE_CURVE('',#1399,#1400,#993,.T.);
#1707=EDGE_CURVE('',#1400,#1398,#994,.T.);
#1708=EDGE_CURVE('',#1399,#1401,#995,.T.);
#1709=EDGE_CURVE('',#1401,#1402,#996,.T.);
#1710=EDGE_CURVE('',#1402,#1400,#997,.T.);
#1711=EDGE_CURVE('',#1401,#1391,#998,.T.);
#1712=EDGE_CURVE('',#1394,#1402,#999,.T.);
#1713=EDGE_CURVE('',#1403,#1403,#370,.T.);
#1714=EDGE_CURVE('',#1404,#1404,#371,.T.);
#1715=EDGE_CURVE('',#1405,#1405,#372,.T.);
#1716=EDGE_CURVE('',#1405,#1404,#1000,.T.);
#1717=EDGE_CURVE('',#1406,#1406,#373,.T.);
#1718=EDGE_CURVE('',#1406,#1405,#1001,.T.);
#1719=EDGE_CURVE('',#1407,#1407,#374,.T.);
#1720=EDGE_CURVE('',#1407,#1406,#1002,.T.);
#1721=EDGE_CURVE('',#1408,#1408,#375,.T.);
#1722=EDGE_CURVE('',#1409,#1409,#376,.F.);
#1723=EDGE_CURVE('',#1409,#1408,#1003,.T.);
#1724=EDGE_CURVE('',#1403,#1409,#1004,.T.);
#1725=EDGE_CURVE('',#1410,#1410,#377,.T.);
#1726=EDGE_CURVE('',#1410,#1411,#1005,.T.);
#1727=EDGE_CURVE('',#1411,#1411,#378,.T.);
#1728=EDGE_CURVE('',#1412,#1412,#379,.T.);
#1729=EDGE_CURVE('',#1412,#1413,#1006,.T.);
#1730=EDGE_CURVE('',#1413,#1413,#380,.T.);
#1731=EDGE_CURVE('',#1414,#1414,#381,.F.);
#1732=EDGE_CURVE('',#1414,#1415,#1007,.T.);
#1733=EDGE_CURVE('',#1415,#1415,#382,.F.);
#1734=EDGE_CURVE('',#1416,#1416,#383,.T.);
#1735=EDGE_CURVE('',#1416,#1414,#1008,.T.);
#1736=EDGE_CURVE('',#1417,#1417,#384,.T.);
#1737=EDGE_CURVE('',#1417,#1418,#1009,.T.);
#1738=EDGE_CURVE('',#1419,#1418,#141,.T.);
#1739=EDGE_CURVE('',#1420,#1419,#142,.T.);
#1740=EDGE_CURVE('',#1421,#1420,#143,.T.);
#1741=EDGE_CURVE('',#1422,#1421,#144,.T.);
#1742=EDGE_CURVE('',#1423,#1422,#145,.T.);
#1743=EDGE_CURVE('',#1418,#1423,#146,.T.);
#1744=EDGE_CURVE('',#1424,#1422,#1010,.T.);
#1745=EDGE_CURVE('',#1424,#1425,#1011,.T.);
#1746=EDGE_CURVE('',#1425,#1423,#1012,.T.);
#1747=EDGE_CURVE('',#1426,#1421,#1013,.T.);
#1748=EDGE_CURVE('',#1426,#1424,#1014,.T.);
#1749=EDGE_CURVE('',#1427,#1420,#1015,.T.);
#1750=EDGE_CURVE('',#1427,#1426,#1016,.T.);
#1751=EDGE_CURVE('',#1428,#1419,#1017,.T.);
#1752=EDGE_CURVE('',#1428,#1427,#1018,.T.);
#1753=EDGE_CURVE('',#1429,#1418,#1019,.T.);
#1754=EDGE_CURVE('',#1429,#1428,#1020,.T.);
#1755=EDGE_CURVE('',#1425,#1429,#1021,.T.);
#1756=EDGE_CURVE('',#1430,#1431,#147,.T.);
#1757=EDGE_CURVE('',#1432,#1430,#148,.T.);
#1758=EDGE_CURVE('',#1432,#1433,#1022,.T.);
#1759=EDGE_CURVE('',#1433,#1433,#385,.T.);
#1760=EDGE_CURVE('',#1434,#1432,#149,.T.);
#1761=EDGE_CURVE('',#1435,#1434,#150,.T.);
#1762=EDGE_CURVE('',#1436,#1435,#151,.T.);
#1763=EDGE_CURVE('',#1431,#1436,#152,.T.);
#1764=EDGE_CURVE('',#1437,#1437,#386,.T.);
#1765=EDGE_CURVE('',#1437,#1438,#1023,.T.);
#1766=EDGE_CURVE('',#1439,#1438,#153,.T.);
#1767=EDGE_CURVE('',#1440,#1439,#154,.T.);
#1768=EDGE_CURVE('',#1441,#1440,#155,.T.);
#1769=EDGE_CURVE('',#1442,#1441,#156,.T.);
#1770=EDGE_CURVE('',#1443,#1442,#157,.T.);
#1771=EDGE_CURVE('',#1438,#1443,#158,.T.);
#1772=EDGE_CURVE('',#1434,#1443,#1024,.T.);
#1773=EDGE_CURVE('',#1435,#1442,#1025,.T.);
#1774=EDGE_CURVE('',#1432,#1438,#1026,.T.);
#1775=EDGE_CURVE('',#1430,#1439,#1027,.T.);
#1776=EDGE_CURVE('',#1444,#1444,#387,.F.);
#1777=EDGE_CURVE('',#1444,#1445,#1028,.T.);
#1778=EDGE_CURVE('',#1445,#1445,#388,.F.);
#1779=EDGE_CURVE('',#1431,#1440,#1029,.T.);
#1780=EDGE_CURVE('',#1436,#1441,#1030,.T.);
#1781=EDGE_CURVE('',#1446,#1446,#389,.T.);
#1782=EDGE_CURVE('',#1446,#1447,#1031,.T.);
#1783=EDGE_CURVE('',#1447,#1447,#390,.T.);
#1784=EDGE_CURVE('',#1448,#1448,#391,.T.);
#1785=EDGE_CURVE('',#1449,#1449,#392,.T.);
#1786=EDGE_CURVE('',#1449,#1450,#1032,.T.);
#1787=EDGE_CURVE('',#1450,#1450,#393,.T.);
#1788=EDGE_CURVE('',#1451,#1451,#394,.T.);
#1789=EDGE_CURVE('',#1451,#1448,#1033,.T.);
#1790=EDGE_CURVE('',#1452,#1452,#395,.T.);
#1791=EDGE_CURVE('',#1452,#1453,#1034,.T.);
#1792=EDGE_CURVE('',#1453,#1453,#396,.T.);
#1793=EDGE_CURVE('',#1454,#1455,#397,.T.);
#1794=EDGE_CURVE('',#1455,#1454,#398,.T.);
#1795=EDGE_CURVE('',#1455,#1456,#399,.T.);
#1796=EDGE_CURVE('',#1457,#1456,#400,.T.);
#1797=EDGE_CURVE('',#1456,#1457,#401,.T.);
#1798=EDGE_CURVE('',#1457,#1458,#1035,.T.);
#1799=EDGE_CURVE('',#1458,#1458,#402,.T.);
#1800=EDGE_CURVE('',#1459,#1459,#403,.T.);
#1801=EDGE_CURVE('',#1459,#1460,#1036,.T.);
#1802=EDGE_CURVE('',#1460,#1460,#404,.T.);
#1803=EDGE_CURVE('',#1460,#1461,#1037,.T.);
#1804=EDGE_CURVE('',#1461,#1461,#405,.T.);
#1805=EDGE_CURVE('',#1462,#1462,#406,.T.);
#1806=EDGE_CURVE('',#1462,#1454,#1038,.T.);
#1807=EDGE_CURVE('',#1463,#1463,#407,.T.);
#1808=EDGE_CURVE('',#1463,#1459,#1039,.T.);
#1809=EDGE_CURVE('',#1464,#1465,#408,.T.);
#1810=EDGE_CURVE('',#1465,#1464,#409,.T.);
#1811=EDGE_CURVE('',#1465,#1466,#410,.T.);
#1812=EDGE_CURVE('',#1467,#1466,#411,.T.);
#1813=EDGE_CURVE('',#1466,#1467,#412,.T.);
#1814=EDGE_CURVE('',#1468,#1468,#413,.T.);
#1815=EDGE_CURVE('',#1468,#1467,#1040,.T.);
#1816=EDGE_CURVE('',#1469,#1469,#414,.T.);
#1817=EDGE_CURVE('',#1470,#1470,#415,.T.);
#1818=EDGE_CURVE('',#1471,#1471,#416,.T.);
#1819=EDGE_CURVE('',#1471,#1469,#1041,.T.);
#1820=EDGE_CURVE('',#1472,#1472,#417,.T.);
#1821=EDGE_CURVE('',#1472,#1471,#1042,.T.);
#1822=EDGE_CURVE('',#1473,#1473,#418,.T.);
#1823=EDGE_CURVE('',#1473,#1472,#1043,.T.);
#1824=EDGE_CURVE('',#1464,#1470,#1044,.T.);
#1825=EDGE_CURVE('',#1474,#1475,#419,.T.);
#1826=EDGE_CURVE('',#1476,#1477,#420,.T.);
#1827=EDGE_CURVE('',#1478,#1479,#421,.T.);
#1828=EDGE_CURVE('',#1480,#1481,#422,.T.);
#1829=EDGE_CURVE('',#1482,#1483,#423,.T.);
#1830=EDGE_CURVE('',#1484,#1485,#424,.T.);
#1831=EDGE_CURVE('',#1486,#1487,#425,.T.);
#1832=EDGE_CURVE('',#1488,#1489,#11,.T.);
#1833=EDGE_CURVE('',#1490,#1488,#426,.T.);
#1834=EDGE_CURVE('',#1491,#1490,#12,.T.);
#1835=EDGE_CURVE('',#1489,#1491,#427,.T.);
#1836=EDGE_CURVE('',#1492,#1490,#428,.T.);
#1837=EDGE_CURVE('',#1492,#1493,#13,.T.);
#1838=EDGE_CURVE('',#1494,#1493,#429,.T.);
#1839=EDGE_CURVE('',#1494,#1495,#14,.T.);
#1840=EDGE_CURVE('',#1496,#1495,#430,.T.);
#1841=EDGE_CURVE('',#1496,#1497,#1045,.T.);
#1842=EDGE_CURVE('',#1497,#1497,#431,.T.);
#1843=EDGE_CURVE('',#1498,#1496,#432,.T.);
#1844=EDGE_CURVE('',#1498,#1499,#15,.T.);
#1845=EDGE_CURVE('',#1500,#1499,#433,.T.);
#1846=EDGE_CURVE('',#1500,#1501,#16,.T.);
#1847=EDGE_CURVE('',#1502,#1501,#434,.T.);
#1848=EDGE_CURVE('',#1502,#1503,#17,.T.);
#1849=EDGE_CURVE('',#1504,#1503,#435,.T.);
#1850=EDGE_CURVE('',#1504,#1505,#18,.T.);
#1851=EDGE_CURVE('',#1491,#1505,#436,.T.);
#1852=EDGE_CURVE('',#1488,#1506,#437,.T.);
#1853=EDGE_CURVE('',#1506,#1492,#438,.T.);
#1854=EDGE_CURVE('',#1507,#1506,#19,.T.);
#1855=EDGE_CURVE('',#1493,#1507,#439,.T.);
#1856=EDGE_CURVE('',#1507,#1508,#440,.T.);
#1857=EDGE_CURVE('',#1508,#1494,#441,.T.);
#1858=EDGE_CURVE('',#1509,#1508,#20,.T.);
#1859=EDGE_CURVE('',#1495,#1509,#442,.T.);
#1860=EDGE_CURVE('',#1509,#1510,#443,.T.);
#1861=EDGE_CURVE('',#1510,#1511,#444,.T.);
#1862=EDGE_CURVE('',#1511,#1498,#445,.T.);
#1863=EDGE_CURVE('',#1512,#1511,#21,.T.);
#1864=EDGE_CURVE('',#1499,#1512,#446,.T.);
#1865=EDGE_CURVE('',#1512,#1513,#447,.T.);
#1866=EDGE_CURVE('',#1513,#1500,#448,.T.);
#1867=EDGE_CURVE('',#1514,#1513,#22,.T.);
#1868=EDGE_CURVE('',#1501,#1514,#449,.T.);
#1869=EDGE_CURVE('',#1514,#1515,#450,.T.);
#1870=EDGE_CURVE('',#1515,#1502,#451,.T.);
#1871=EDGE_CURVE('',#1516,#1515,#23,.T.);
#1872=EDGE_CURVE('',#1503,#1516,#452,.T.);
#1873=EDGE_CURVE('',#1517,#1517,#453,.T.);
#1874=EDGE_CURVE('',#1517,#1510,#1046,.T.);
#1875=EDGE_CURVE('',#1518,#1489,#454,.T.);
#1876=EDGE_CURVE('',#1518,#1519,#24,.T.);
#1877=EDGE_CURVE('',#1516,#1519,#455,.T.);
#1878=EDGE_CURVE('',#1505,#1518,#456,.T.);
#1879=EDGE_CURVE('',#1519,#1504,#457,.T.);
#1880=EDGE_CURVE('',#1520,#1520,#458,.T.);
#1881=EDGE_CURVE('',#1521,#1521,#459,.T.);
#1882=EDGE_CURVE('',#1522,#1522,#460,.T.);
#1883=EDGE_CURVE('',#1522,#1520,#1047,.T.);
#1884=EDGE_CURVE('',#1523,#1523,#461,.T.);
#1885=EDGE_CURVE('',#1523,#1521,#1048,.T.);
#1886=EDGE_CURVE('',#1524,#1524,#462,.T.);
#1887=EDGE_CURVE('',#1525,#1525,#463,.T.);
#1888=EDGE_CURVE('',#1526,#1526,#464,.T.);
#1889=EDGE_CURVE('',#1526,#1524,#1049,.T.);
#1890=EDGE_CURVE('',#1527,#1527,#465,.T.);
#1891=EDGE_CURVE('',#1527,#1525,#1050,.T.);
#1892=EDGE_CURVE('',#1528,#1528,#466,.T.);
#1893=EDGE_CURVE('',#1528,#1529,#1051,.T.);
#1894=EDGE_CURVE('',#1529,#1529,#467,.T.);
#1895=EDGE_CURVE('',#1530,#1530,#468,.T.);
#1896=EDGE_CURVE('',#1530,#1531,#1052,.T.);
#1897=EDGE_CURVE('',#1531,#1531,#469,.T.);
#1898=EDGE_CURVE('',#1532,#1532,#470,.T.);
#1899=EDGE_CURVE('',#1532,#1533,#1053,.T.);
#1900=EDGE_CURVE('',#1533,#1533,#471,.T.);
#1901=EDGE_CURVE('',#1534,#1535,#1054,.T.);
#1902=EDGE_CURVE('',#1536,#1534,#1055,.T.);
#1903=EDGE_CURVE('',#1537,#1536,#1056,.T.);
#1904=EDGE_CURVE('',#1535,#1537,#1057,.T.);
#1905=EDGE_CURVE('',#1537,#1538,#1058,.T.);
#1906=EDGE_CURVE('',#1539,#1536,#1059,.T.);
#1907=EDGE_CURVE('',#1538,#1539,#1060,.T.);
#1908=EDGE_CURVE('',#1540,#1541,#1061,.T.);
#1909=EDGE_CURVE('',#1538,#1540,#1062,.T.);
#1910=EDGE_CURVE('',#1541,#1539,#1063,.T.);
#1911=EDGE_CURVE('',#1542,#1540,#472,.T.);
#1912=EDGE_CURVE('',#1542,#1543,#1064,.T.);
#1913=EDGE_CURVE('',#1543,#1544,#1065,.T.);
#1914=EDGE_CURVE('',#1544,#1545,#1066,.T.);
#1915=EDGE_CURVE('',#1545,#1546,#1067,.T.);
#1916=EDGE_CURVE('',#1535,#1546,#473,.T.);
#1917=EDGE_CURVE('',#1547,#1541,#474,.T.);
#1918=EDGE_CURVE('',#1547,#1542,#1068,.T.);
#1919=EDGE_CURVE('',#1546,#1548,#1069,.T.);
#1920=EDGE_CURVE('',#1545,#1549,#1070,.T.);
#1921=EDGE_CURVE('',#1548,#1549,#1071,.T.);
#1922=EDGE_CURVE('',#1550,#1547,#1072,.T.);
#1923=EDGE_CURVE('',#1543,#1550,#1073,.T.);
#1924=EDGE_CURVE('',#1551,#1550,#1074,.T.);
#1925=EDGE_CURVE('',#1544,#1551,#1075,.T.);
#1926=EDGE_CURVE('',#1549,#1551,#1076,.T.);
#1927=EDGE_CURVE('',#1534,#1548,#475,.T.);
#1928=EDGE_CURVE('',#1552,#1553,#1077,.T.);
#1929=EDGE_CURVE('',#1553,#1554,#1078,.T.);
#1930=EDGE_CURVE('',#1555,#1554,#1079,.T.);
#1931=EDGE_CURVE('',#1552,#1555,#1080,.T.);
#1932=EDGE_CURVE('',#1556,#1552,#1081,.T.);
#1933=EDGE_CURVE('',#1557,#1555,#1082,.T.);
#1934=EDGE_CURVE('',#1556,#1557,#1083,.T.);
#1935=EDGE_CURVE('',#1558,#1556,#1084,.T.);
#1936=EDGE_CURVE('',#1559,#1557,#1085,.T.);
#1937=EDGE_CURVE('',#1558,#1559,#1086,.T.);
#1938=EDGE_CURVE('',#1553,#1558,#1087,.T.);
#1939=EDGE_CURVE('',#1554,#1559,#1088,.T.);
#1940=ORIENTED_EDGE('',*,*,#1560,.F.);
#1941=ORIENTED_EDGE('',*,*,#1561,.F.);
#1942=ORIENTED_EDGE('',*,*,#1562,.F.);
#1943=ORIENTED_EDGE('',*,*,#1563,.T.);
#1944=ORIENTED_EDGE('',*,*,#1564,.F.);
#1945=ORIENTED_EDGE('',*,*,#1565,.F.);
#1946=ORIENTED_EDGE('',*,*,#1566,.F.);
#1947=ORIENTED_EDGE('',*,*,#1567,.F.);
#1948=ORIENTED_EDGE('',*,*,#1568,.F.);
#1949=ORIENTED_EDGE('',*,*,#1569,.F.);
#1950=ORIENTED_EDGE('',*,*,#1570,.F.);
#1951=ORIENTED_EDGE('',*,*,#1561,.T.);
#1952=ORIENTED_EDGE('',*,*,#1571,.F.);
#1953=ORIENTED_EDGE('',*,*,#1572,.F.);
#1954=ORIENTED_EDGE('',*,*,#1573,.F.);
#1955=ORIENTED_EDGE('',*,*,#1568,.T.);
#1956=ORIENTED_EDGE('',*,*,#1574,.F.);
#1957=ORIENTED_EDGE('',*,*,#1575,.T.);
#1958=ORIENTED_EDGE('',*,*,#1576,.F.);
#1959=ORIENTED_EDGE('',*,*,#1577,.F.);
#1960=ORIENTED_EDGE('',*,*,#1578,.F.);
#1961=ORIENTED_EDGE('',*,*,#1563,.F.);
#1962=ORIENTED_EDGE('',*,*,#1579,.F.);
#1963=ORIENTED_EDGE('',*,*,#1580,.F.);
#1964=ORIENTED_EDGE('',*,*,#1575,.F.);
#1965=ORIENTED_EDGE('',*,*,#1581,.F.);
#1966=ORIENTED_EDGE('',*,*,#1582,.F.);
#1967=ORIENTED_EDGE('',*,*,#1583,.T.);
#1968=ORIENTED_EDGE('',*,*,#1584,.F.);
#1969=ORIENTED_EDGE('',*,*,#1583,.F.);
#1970=ORIENTED_EDGE('',*,*,#1585,.F.);
#1971=ORIENTED_EDGE('',*,*,#1565,.T.);
#1972=ORIENTED_EDGE('',*,*,#1577,.T.);
#1973=ORIENTED_EDGE('',*,*,#1586,.T.);
#1974=ORIENTED_EDGE('',*,*,#1587,.T.);
#1975=ORIENTED_EDGE('',*,*,#1588,.T.);
#1976=ORIENTED_EDGE('',*,*,#1589,.T.);
#1977=ORIENTED_EDGE('',*,*,#1576,.T.);
#1978=ORIENTED_EDGE('',*,*,#1580,.T.);
#1979=ORIENTED_EDGE('',*,*,#1590,.F.);
#1980=ORIENTED_EDGE('',*,*,#1591,.F.);
#1981=ORIENTED_EDGE('',*,*,#1592,.F.);
#1982=ORIENTED_EDGE('',*,*,#1586,.F.);
#1983=ORIENTED_EDGE('',*,*,#1569,.T.);
#1984=ORIENTED_EDGE('',*,*,#1573,.T.);
#1985=ORIENTED_EDGE('',*,*,#1593,.F.);
#1986=ORIENTED_EDGE('',*,*,#1594,.F.);
#1987=ORIENTED_EDGE('',*,*,#1595,.F.);
#1988=ORIENTED_EDGE('',*,*,#1596,.F.);
#1989=ORIENTED_EDGE('',*,*,#1597,.F.);
#1990=ORIENTED_EDGE('',*,*,#1598,.T.);
#1991=ORIENTED_EDGE('',*,*,#1599,.F.);
#1992=ORIENTED_EDGE('',*,*,#1598,.F.);
#1993=ORIENTED_EDGE('',*,*,#1589,.F.);
#1994=ORIENTED_EDGE('',*,*,#1600,.T.);
#1995=ORIENTED_EDGE('',*,*,#1601,.F.);
#1996=ORIENTED_EDGE('',*,*,#1600,.F.);
#1997=ORIENTED_EDGE('',*,*,#1602,.F.);
#1998=ORIENTED_EDGE('',*,*,#1603,.T.);
#1999=ORIENTED_EDGE('',*,*,#1604,.T.);
#2000=ORIENTED_EDGE('',*,*,#1591,.T.);
#2001=ORIENTED_EDGE('',*,*,#1601,.T.);
#2002=ORIENTED_EDGE('',*,*,#1574,.T.);
#2003=ORIENTED_EDGE('',*,*,#1588,.F.);
#2004=ORIENTED_EDGE('',*,*,#1605,.T.);
#2005=ORIENTED_EDGE('',*,*,#1603,.F.);
#2006=ORIENTED_EDGE('',*,*,#1606,.F.);
#2007=ORIENTED_EDGE('',*,*,#1581,.T.);
#2008=ORIENTED_EDGE('',*,*,#1587,.F.);
#2009=ORIENTED_EDGE('',*,*,#1592,.T.);
#2010=ORIENTED_EDGE('',*,*,#1604,.F.);
#2011=ORIENTED_EDGE('',*,*,#1605,.F.);
#2012=ORIENTED_EDGE('',*,*,#1572,.T.);
#2013=ORIENTED_EDGE('',*,*,#1607,.T.);
#2014=ORIENTED_EDGE('',*,*,#1608,.T.);
#2015=ORIENTED_EDGE('',*,*,#1593,.T.);
#2016=ORIENTED_EDGE('',*,*,#1599,.T.);
#2017=ORIENTED_EDGE('',*,*,#1567,.T.);
#2018=ORIENTED_EDGE('',*,*,#1609,.F.);
#2019=ORIENTED_EDGE('',*,*,#1610,.F.);
#2020=ORIENTED_EDGE('',*,*,#1611,.T.);
#2021=ORIENTED_EDGE('',*,*,#1607,.F.);
#2022=ORIENTED_EDGE('',*,*,#1571,.T.);
#2023=ORIENTED_EDGE('',*,*,#1612,.F.);
#2024=ORIENTED_EDGE('',*,*,#1594,.T.);
#2025=ORIENTED_EDGE('',*,*,#1608,.F.);
#2026=ORIENTED_EDGE('',*,*,#1611,.F.);
#2027=ORIENTED_EDGE('',*,*,#1613,.F.);
#2028=ORIENTED_EDGE('',*,*,#1595,.T.);
#2029=ORIENTED_EDGE('',*,*,#1612,.T.);
#2030=ORIENTED_EDGE('',*,*,#1610,.T.);
#2031=ORIENTED_EDGE('',*,*,#1597,.T.);
#2032=ORIENTED_EDGE('',*,*,#1614,.F.);
#2033=ORIENTED_EDGE('',*,*,#1615,.F.);
#2034=ORIENTED_EDGE('',*,*,#1616,.F.);
#2035=ORIENTED_EDGE('',*,*,#1617,.F.);
#2036=ORIENTED_EDGE('',*,*,#1618,.F.);
#2037=ORIENTED_EDGE('',*,*,#1619,.F.);
#2038=ORIENTED_EDGE('',*,*,#1620,.F.);
#2039=ORIENTED_EDGE('',*,*,#1621,.F.);
#2040=ORIENTED_EDGE('',*,*,#1620,.T.);
#2041=ORIENTED_EDGE('',*,*,#1622,.T.);
#2042=ORIENTED_EDGE('',*,*,#1623,.T.);
#2043=ORIENTED_EDGE('',*,*,#1624,.F.);
#2044=ORIENTED_EDGE('',*,*,#1625,.T.);
#2045=ORIENTED_EDGE('',*,*,#1626,.T.);
#2046=ORIENTED_EDGE('',*,*,#1619,.T.);
#2047=ORIENTED_EDGE('',*,*,#1627,.F.);
#2048=ORIENTED_EDGE('',*,*,#1628,.F.);
#2049=ORIENTED_EDGE('',*,*,#1622,.F.);
#2050=ORIENTED_EDGE('',*,*,#1616,.T.);
#2051=ORIENTED_EDGE('',*,*,#1629,.T.);
#2052=ORIENTED_EDGE('',*,*,#1630,.T.);
#2053=ORIENTED_EDGE('',*,*,#1631,.F.);
#2054=ORIENTED_EDGE('',*,*,#1632,.T.);
#2055=ORIENTED_EDGE('',*,*,#1633,.T.);
#2056=ORIENTED_EDGE('',*,*,#1615,.T.);
#2057=ORIENTED_EDGE('',*,*,#1634,.F.);
#2058=ORIENTED_EDGE('',*,*,#1635,.F.);
#2059=ORIENTED_EDGE('',*,*,#1629,.F.);
#2060=ORIENTED_EDGE('',*,*,#1618,.T.);
#2061=ORIENTED_EDGE('',*,*,#1636,.T.);
#2062=ORIENTED_EDGE('',*,*,#1637,.T.);
#2063=ORIENTED_EDGE('',*,*,#1638,.F.);
#2064=ORIENTED_EDGE('',*,*,#1639,.T.);
#2065=ORIENTED_EDGE('',*,*,#1627,.T.);
#2066=ORIENTED_EDGE('',*,*,#1640,.F.);
#2067=ORIENTED_EDGE('',*,*,#1623,.F.);
#2068=ORIENTED_EDGE('',*,*,#1628,.T.);
#2069=ORIENTED_EDGE('',*,*,#1639,.F.);
#2070=ORIENTED_EDGE('',*,*,#1641,.F.);
#2071=ORIENTED_EDGE('',*,*,#1637,.F.);
#2072=ORIENTED_EDGE('',*,*,#1642,.F.);
#2073=ORIENTED_EDGE('',*,*,#1625,.F.);
#2074=ORIENTED_EDGE('',*,*,#1621,.T.);
#2075=ORIENTED_EDGE('',*,*,#1626,.F.);
#2076=ORIENTED_EDGE('',*,*,#1642,.T.);
#2077=ORIENTED_EDGE('',*,*,#1636,.F.);
#2078=ORIENTED_EDGE('',*,*,#1614,.T.);
#2079=ORIENTED_EDGE('',*,*,#1643,.T.);
#2080=ORIENTED_EDGE('',*,*,#1644,.T.);
#2081=ORIENTED_EDGE('',*,*,#1645,.F.);
#2082=ORIENTED_EDGE('',*,*,#1646,.T.);
#2083=ORIENTED_EDGE('',*,*,#1634,.T.);
#2084=ORIENTED_EDGE('',*,*,#1647,.F.);
#2085=ORIENTED_EDGE('',*,*,#1630,.F.);
#2086=ORIENTED_EDGE('',*,*,#1635,.T.);
#2087=ORIENTED_EDGE('',*,*,#1646,.F.);
#2088=ORIENTED_EDGE('',*,*,#1648,.F.);
#2089=ORIENTED_EDGE('',*,*,#1644,.F.);
#2090=ORIENTED_EDGE('',*,*,#1649,.F.);
#2091=ORIENTED_EDGE('',*,*,#1632,.F.);
#2092=ORIENTED_EDGE('',*,*,#1617,.T.);
#2093=ORIENTED_EDGE('',*,*,#1633,.F.);
#2094=ORIENTED_EDGE('',*,*,#1649,.T.);
#2095=ORIENTED_EDGE('',*,*,#1643,.F.);
#2096=ORIENTED_EDGE('',*,*,#1650,.F.);
#2097=ORIENTED_EDGE('',*,*,#1651,.T.);
#2098=ORIENTED_EDGE('',*,*,#1652,.F.);
#2099=ORIENTED_EDGE('',*,*,#1651,.F.);
#2100=ORIENTED_EDGE('',*,*,#1653,.F.);
#2101=ORIENTED_EDGE('',*,*,#1654,.T.);
#2102=ORIENTED_EDGE('',*,*,#1655,.F.);
#2103=ORIENTED_EDGE('',*,*,#1654,.F.);
#2104=ORIENTED_EDGE('',*,*,#1656,.F.);
#2105=ORIENTED_EDGE('',*,*,#1657,.T.);
#2106=ORIENTED_EDGE('',*,*,#1658,.F.);
#2107=ORIENTED_EDGE('',*,*,#1657,.F.);
#2108=ORIENTED_EDGE('',*,*,#1659,.F.);
#2109=ORIENTED_EDGE('',*,*,#1660,.T.);
#2110=ORIENTED_EDGE('',*,*,#1661,.F.);
#2111=ORIENTED_EDGE('',*,*,#1660,.F.);
#2112=ORIENTED_EDGE('',*,*,#1662,.T.);
#2113=ORIENTED_EDGE('',*,*,#1663,.T.);
#2114=ORIENTED_EDGE('',*,*,#1664,.F.);
#2115=ORIENTED_EDGE('',*,*,#1665,.F.);
#2116=ORIENTED_EDGE('',*,*,#1666,.T.);
#2117=ORIENTED_EDGE('',*,*,#1665,.T.);
#2118=ORIENTED_EDGE('',*,*,#1667,.F.);
#2119=ORIENTED_EDGE('',*,*,#1668,.F.);
#2120=ORIENTED_EDGE('',*,*,#1669,.T.);
#2121=ORIENTED_EDGE('',*,*,#1668,.T.);
#2122=ORIENTED_EDGE('',*,*,#1670,.F.);
#2123=ORIENTED_EDGE('',*,*,#1671,.F.);
#2124=ORIENTED_EDGE('',*,*,#1672,.T.);
#2125=ORIENTED_EDGE('',*,*,#1671,.T.);
#2126=ORIENTED_EDGE('',*,*,#1673,.F.);
#2127=ORIENTED_EDGE('',*,*,#1663,.F.);
#2128=ORIENTED_EDGE('',*,*,#1673,.T.);
#2129=ORIENTED_EDGE('',*,*,#1670,.T.);
#2130=ORIENTED_EDGE('',*,*,#1667,.T.);
#2131=ORIENTED_EDGE('',*,*,#1664,.T.);
#2132=ORIENTED_EDGE('',*,*,#1578,.T.);
#2133=ORIENTED_EDGE('',*,*,#1584,.T.);
#2134=ORIENTED_EDGE('',*,*,#1564,.T.);
#2135=ORIENTED_EDGE('',*,*,#1560,.T.);
#2136=ORIENTED_EDGE('',*,*,#1652,.T.);
#2137=ORIENTED_EDGE('',*,*,#1655,.T.);
#2138=ORIENTED_EDGE('',*,*,#1658,.T.);
#2139=ORIENTED_EDGE('',*,*,#1661,.T.);
#2140=ORIENTED_EDGE('',*,*,#1672,.F.);
#2141=ORIENTED_EDGE('',*,*,#1662,.F.);
#2142=ORIENTED_EDGE('',*,*,#1666,.F.);
#2143=ORIENTED_EDGE('',*,*,#1669,.F.);
#2144=ORIENTED_EDGE('',*,*,#1582,.T.);
#2145=ORIENTED_EDGE('',*,*,#1606,.T.);
#2146=ORIENTED_EDGE('',*,*,#1602,.T.);
#2147=ORIENTED_EDGE('',*,*,#1590,.T.);
#2148=ORIENTED_EDGE('',*,*,#1579,.T.);
#2149=ORIENTED_EDGE('',*,*,#1562,.T.);
#2150=ORIENTED_EDGE('',*,*,#1570,.T.);
#2151=ORIENTED_EDGE('',*,*,#1596,.T.);
#2152=ORIENTED_EDGE('',*,*,#1613,.T.);
#2153=ORIENTED_EDGE('',*,*,#1609,.T.);
#2154=ORIENTED_EDGE('',*,*,#1566,.T.);
#2155=ORIENTED_EDGE('',*,*,#1585,.T.);
#2156=ORIENTED_EDGE('',*,*,#1659,.T.);
#2157=ORIENTED_EDGE('',*,*,#1656,.T.);
#2158=ORIENTED_EDGE('',*,*,#1653,.T.);
#2159=ORIENTED_EDGE('',*,*,#1650,.T.);
#2160=ORIENTED_EDGE('',*,*,#1647,.T.);
#2161=ORIENTED_EDGE('',*,*,#1645,.T.);
#2162=ORIENTED_EDGE('',*,*,#1648,.T.);
#2163=ORIENTED_EDGE('',*,*,#1631,.T.);
#2164=ORIENTED_EDGE('',*,*,#1640,.T.);
#2165=ORIENTED_EDGE('',*,*,#1638,.T.);
#2166=ORIENTED_EDGE('',*,*,#1641,.T.);
#2167=ORIENTED_EDGE('',*,*,#1624,.T.);
#2168=ORIENTED_EDGE('',*,*,#1674,.F.);
#2169=ORIENTED_EDGE('',*,*,#1675,.T.);
#2170=ORIENTED_EDGE('',*,*,#1676,.F.);
#2171=ORIENTED_EDGE('',*,*,#1675,.F.);
#2172=ORIENTED_EDGE('',*,*,#1674,.T.);
#2173=ORIENTED_EDGE('',*,*,#1677,.T.);
#2174=ORIENTED_EDGE('',*,*,#1678,.F.);
#2175=ORIENTED_EDGE('',*,*,#1677,.F.);
#2176=ORIENTED_EDGE('',*,*,#1679,.T.);
#2177=ORIENTED_EDGE('',*,*,#1680,.T.);
#2178=ORIENTED_EDGE('',*,*,#1679,.F.);
#2179=ORIENTED_EDGE('',*,*,#1680,.F.);
#2180=ORIENTED_EDGE('',*,*,#1681,.F.);
#2181=ORIENTED_EDGE('',*,*,#1682,.T.);
#2182=ORIENTED_EDGE('',*,*,#1678,.T.);
#2183=ORIENTED_EDGE('',*,*,#1682,.F.);
#2184=ORIENTED_EDGE('',*,*,#1681,.T.);
#2185=ORIENTED_EDGE('',*,*,#1676,.T.);
#2186=ORIENTED_EDGE('',*,*,#1683,.F.);
#2187=ORIENTED_EDGE('',*,*,#1684,.T.);
#2188=ORIENTED_EDGE('',*,*,#1685,.T.);
#2189=ORIENTED_EDGE('',*,*,#1684,.F.);
#2190=ORIENTED_EDGE('',*,*,#1686,.F.);
#2191=ORIENTED_EDGE('',*,*,#1687,.T.);
#2192=ORIENTED_EDGE('',*,*,#1688,.T.);
#2193=ORIENTED_EDGE('',*,*,#1687,.F.);
#2194=ORIENTED_EDGE('',*,*,#1686,.T.);
#2195=ORIENTED_EDGE('',*,*,#1683,.T.);
#2196=ORIENTED_EDGE('',*,*,#1688,.F.);
#2197=ORIENTED_EDGE('',*,*,#1685,.F.);
#2198=ORIENTED_EDGE('',*,*,#1689,.F.);
#2199=ORIENTED_EDGE('',*,*,#1690,.T.);
#2200=ORIENTED_EDGE('',*,*,#1691,.T.);
#2201=ORIENTED_EDGE('',*,*,#1690,.F.);
#2202=ORIENTED_EDGE('',*,*,#1692,.F.);
#2203=ORIENTED_EDGE('',*,*,#1693,.T.);
#2204=ORIENTED_EDGE('',*,*,#1694,.T.);
#2205=ORIENTED_EDGE('',*,*,#1693,.F.);
#2206=ORIENTED_EDGE('',*,*,#1692,.T.);
#2207=ORIENTED_EDGE('',*,*,#1689,.T.);
#2208=ORIENTED_EDGE('',*,*,#1694,.F.);
#2209=ORIENTED_EDGE('',*,*,#1691,.F.);
#2210=ORIENTED_EDGE('',*,*,#1695,.T.);
#2211=ORIENTED_EDGE('',*,*,#1696,.T.);
#2212=ORIENTED_EDGE('',*,*,#1697,.T.);
#2213=ORIENTED_EDGE('',*,*,#1698,.F.);
#2214=ORIENTED_EDGE('',*,*,#1699,.T.);
#2215=ORIENTED_EDGE('',*,*,#1700,.T.);
#2216=ORIENTED_EDGE('',*,*,#1701,.T.);
#2217=ORIENTED_EDGE('',*,*,#1696,.F.);
#2218=ORIENTED_EDGE('',*,*,#1702,.T.);
#2219=ORIENTED_EDGE('',*,*,#1703,.T.);
#2220=ORIENTED_EDGE('',*,*,#1704,.T.);
#2221=ORIENTED_EDGE('',*,*,#1700,.F.);
#2222=ORIENTED_EDGE('',*,*,#1705,.T.);
#2223=ORIENTED_EDGE('',*,*,#1706,.T.);
#2224=ORIENTED_EDGE('',*,*,#1707,.T.);
#2225=ORIENTED_EDGE('',*,*,#1703,.F.);
#2226=ORIENTED_EDGE('',*,*,#1708,.T.);
#2227=ORIENTED_EDGE('',*,*,#1709,.T.);
#2228=ORIENTED_EDGE('',*,*,#1710,.T.);
#2229=ORIENTED_EDGE('',*,*,#1706,.F.);
#2230=ORIENTED_EDGE('',*,*,#1711,.T.);
#2231=ORIENTED_EDGE('',*,*,#1698,.T.);
#2232=ORIENTED_EDGE('',*,*,#1712,.T.);
#2233=ORIENTED_EDGE('',*,*,#1709,.F.);
#2234=ORIENTED_EDGE('',*,*,#1711,.F.);
#2235=ORIENTED_EDGE('',*,*,#1708,.F.);
#2236=ORIENTED_EDGE('',*,*,#1705,.F.);
#2237=ORIENTED_EDGE('',*,*,#1702,.F.);
#2238=ORIENTED_EDGE('',*,*,#1699,.F.);
#2239=ORIENTED_EDGE('',*,*,#1695,.F.);
#2240=ORIENTED_EDGE('',*,*,#1712,.F.);
#2241=ORIENTED_EDGE('',*,*,#1697,.F.);
#2242=ORIENTED_EDGE('',*,*,#1701,.F.);
#2243=ORIENTED_EDGE('',*,*,#1704,.F.);
#2244=ORIENTED_EDGE('',*,*,#1707,.F.);
#2245=ORIENTED_EDGE('',*,*,#1710,.F.);
#2246=ORIENTED_EDGE('',*,*,#1713,.F.);
#2247=ORIENTED_EDGE('',*,*,#1714,.F.);
#2248=ORIENTED_EDGE('',*,*,#1715,.F.);
#2249=ORIENTED_EDGE('',*,*,#1716,.T.);
#2250=ORIENTED_EDGE('',*,*,#1714,.T.);
#2251=ORIENTED_EDGE('',*,*,#1716,.F.);
#2252=ORIENTED_EDGE('',*,*,#1717,.F.);
#2253=ORIENTED_EDGE('',*,*,#1718,.T.);
#2254=ORIENTED_EDGE('',*,*,#1715,.T.);
#2255=ORIENTED_EDGE('',*,*,#1718,.F.);
#2256=ORIENTED_EDGE('',*,*,#1719,.F.);
#2257=ORIENTED_EDGE('',*,*,#1720,.T.);
#2258=ORIENTED_EDGE('',*,*,#1717,.T.);
#2259=ORIENTED_EDGE('',*,*,#1720,.F.);
#2260=ORIENTED_EDGE('',*,*,#1719,.T.);
#2261=ORIENTED_EDGE('',*,*,#1721,.F.);
#2262=ORIENTED_EDGE('',*,*,#1722,.F.);
#2263=ORIENTED_EDGE('',*,*,#1723,.T.);
#2264=ORIENTED_EDGE('',*,*,#1721,.T.);
#2265=ORIENTED_EDGE('',*,*,#1723,.F.);
#2266=ORIENTED_EDGE('',*,*,#1713,.T.);
#2267=ORIENTED_EDGE('',*,*,#1724,.T.);
#2268=ORIENTED_EDGE('',*,*,#1722,.T.);
#2269=ORIENTED_EDGE('',*,*,#1724,.F.);
#2270=ORIENTED_EDGE('',*,*,#1725,.F.);
#2271=ORIENTED_EDGE('',*,*,#1726,.T.);
#2272=ORIENTED_EDGE('',*,*,#1727,.T.);
#2273=ORIENTED_EDGE('',*,*,#1726,.F.);
#2274=ORIENTED_EDGE('',*,*,#1728,.F.);
#2275=ORIENTED_EDGE('',*,*,#1729,.T.);
#2276=ORIENTED_EDGE('',*,*,#1730,.T.);
#2277=ORIENTED_EDGE('',*,*,#1729,.F.);
#2278=ORIENTED_EDGE('',*,*,#1728,.T.);
#2279=ORIENTED_EDGE('',*,*,#1725,.T.);
#2280=ORIENTED_EDGE('',*,*,#1730,.F.);
#2281=ORIENTED_EDGE('',*,*,#1727,.F.);
#2282=ORIENTED_EDGE('',*,*,#1731,.F.);
#2283=ORIENTED_EDGE('',*,*,#1732,.T.);
#2284=ORIENTED_EDGE('',*,*,#1733,.F.);
#2285=ORIENTED_EDGE('',*,*,#1732,.F.);
#2286=ORIENTED_EDGE('',*,*,#1734,.F.);
#2287=ORIENTED_EDGE('',*,*,#1735,.T.);
#2288=ORIENTED_EDGE('',*,*,#1731,.T.);
#2289=ORIENTED_EDGE('',*,*,#1735,.F.);
#2290=ORIENTED_EDGE('',*,*,#1734,.T.);
#2291=ORIENTED_EDGE('',*,*,#1736,.F.);
#2292=ORIENTED_EDGE('',*,*,#1737,.T.);
#2293=ORIENTED_EDGE('',*,*,#1738,.F.);
#2294=ORIENTED_EDGE('',*,*,#1739,.F.);
#2295=ORIENTED_EDGE('',*,*,#1740,.F.);
#2296=ORIENTED_EDGE('',*,*,#1741,.F.);
#2297=ORIENTED_EDGE('',*,*,#1742,.F.);
#2298=ORIENTED_EDGE('',*,*,#1743,.F.);
#2299=ORIENTED_EDGE('',*,*,#1737,.F.);
#2300=ORIENTED_EDGE('',*,*,#1742,.T.);
#2301=ORIENTED_EDGE('',*,*,#1744,.F.);
#2302=ORIENTED_EDGE('',*,*,#1745,.T.);
#2303=ORIENTED_EDGE('',*,*,#1746,.T.);
#2304=ORIENTED_EDGE('',*,*,#1741,.T.);
#2305=ORIENTED_EDGE('',*,*,#1747,.F.);
#2306=ORIENTED_EDGE('',*,*,#1748,.T.);
#2307=ORIENTED_EDGE('',*,*,#1744,.T.);
#2308=ORIENTED_EDGE('',*,*,#1740,.T.);
#2309=ORIENTED_EDGE('',*,*,#1749,.F.);
#2310=ORIENTED_EDGE('',*,*,#1750,.T.);
#2311=ORIENTED_EDGE('',*,*,#1747,.T.);
#2312=ORIENTED_EDGE('',*,*,#1739,.T.);
#2313=ORIENTED_EDGE('',*,*,#1751,.F.);
#2314=ORIENTED_EDGE('',*,*,#1752,.T.);
#2315=ORIENTED_EDGE('',*,*,#1749,.T.);
#2316=ORIENTED_EDGE('',*,*,#1738,.T.);
#2317=ORIENTED_EDGE('',*,*,#1753,.F.);
#2318=ORIENTED_EDGE('',*,*,#1754,.T.);
#2319=ORIENTED_EDGE('',*,*,#1751,.T.);
#2320=ORIENTED_EDGE('',*,*,#1743,.T.);
#2321=ORIENTED_EDGE('',*,*,#1746,.F.);
#2322=ORIENTED_EDGE('',*,*,#1755,.T.);
#2323=ORIENTED_EDGE('',*,*,#1753,.T.);
#2324=ORIENTED_EDGE('',*,*,#1736,.T.);
#2325=ORIENTED_EDGE('',*,*,#1750,.F.);
#2326=ORIENTED_EDGE('',*,*,#1752,.F.);
#2327=ORIENTED_EDGE('',*,*,#1754,.F.);
#2328=ORIENTED_EDGE('',*,*,#1755,.F.);
#2329=ORIENTED_EDGE('',*,*,#1745,.F.);
#2330=ORIENTED_EDGE('',*,*,#1748,.F.);
#2331=ORIENTED_EDGE('',*,*,#1733,.T.);
#2332=ORIENTED_EDGE('',*,*,#1756,.F.);
#2333=ORIENTED_EDGE('',*,*,#1757,.F.);
#2334=ORIENTED_EDGE('',*,*,#1758,.T.);
#2335=ORIENTED_EDGE('',*,*,#1759,.F.);
#2336=ORIENTED_EDGE('',*,*,#1758,.F.);
#2337=ORIENTED_EDGE('',*,*,#1760,.F.);
#2338=ORIENTED_EDGE('',*,*,#1761,.F.);
#2339=ORIENTED_EDGE('',*,*,#1762,.F.);
#2340=ORIENTED_EDGE('',*,*,#1763,.F.);
#2341=ORIENTED_EDGE('',*,*,#1764,.F.);
#2342=ORIENTED_EDGE('',*,*,#1765,.T.);
#2343=ORIENTED_EDGE('',*,*,#1766,.F.);
#2344=ORIENTED_EDGE('',*,*,#1767,.F.);
#2345=ORIENTED_EDGE('',*,*,#1768,.F.);
#2346=ORIENTED_EDGE('',*,*,#1769,.F.);
#2347=ORIENTED_EDGE('',*,*,#1770,.F.);
#2348=ORIENTED_EDGE('',*,*,#1771,.F.);
#2349=ORIENTED_EDGE('',*,*,#1765,.F.);
#2350=ORIENTED_EDGE('',*,*,#1761,.T.);
#2351=ORIENTED_EDGE('',*,*,#1772,.T.);
#2352=ORIENTED_EDGE('',*,*,#1770,.T.);
#2353=ORIENTED_EDGE('',*,*,#1773,.F.);
#2354=ORIENTED_EDGE('',*,*,#1760,.T.);
#2355=ORIENTED_EDGE('',*,*,#1774,.T.);
#2356=ORIENTED_EDGE('',*,*,#1771,.T.);
#2357=ORIENTED_EDGE('',*,*,#1772,.F.);
#2358=ORIENTED_EDGE('',*,*,#1757,.T.);
#2359=ORIENTED_EDGE('',*,*,#1775,.T.);
#2360=ORIENTED_EDGE('',*,*,#1766,.T.);
#2361=ORIENTED_EDGE('',*,*,#1774,.F.);
#2362=ORIENTED_EDGE('',*,*,#1776,.F.);
#2363=ORIENTED_EDGE('',*,*,#1777,.T.);
#2364=ORIENTED_EDGE('',*,*,#1778,.T.);
#2365=ORIENTED_EDGE('',*,*,#1777,.F.);
#2366=ORIENTED_EDGE('',*,*,#1756,.T.);
#2367=ORIENTED_EDGE('',*,*,#1779,.T.);
#2368=ORIENTED_EDGE('',*,*,#1767,.T.);
#2369=ORIENTED_EDGE('',*,*,#1775,.F.);
#2370=ORIENTED_EDGE('',*,*,#1762,.T.);
#2371=ORIENTED_EDGE('',*,*,#1773,.T.);
#2372=ORIENTED_EDGE('',*,*,#1769,.T.);
#2373=ORIENTED_EDGE('',*,*,#1780,.F.);
#2374=ORIENTED_EDGE('',*,*,#1763,.T.);
#2375=ORIENTED_EDGE('',*,*,#1780,.T.);
#2376=ORIENTED_EDGE('',*,*,#1768,.T.);
#2377=ORIENTED_EDGE('',*,*,#1779,.F.);
#2378=ORIENTED_EDGE('',*,*,#1764,.T.);
#2379=ORIENTED_EDGE('',*,*,#1776,.T.);
#2380=ORIENTED_EDGE('',*,*,#1759,.T.);
#2381=ORIENTED_EDGE('',*,*,#1778,.F.);
#2382=ORIENTED_EDGE('',*,*,#1781,.F.);
#2383=ORIENTED_EDGE('',*,*,#1782,.T.);
#2384=ORIENTED_EDGE('',*,*,#1783,.F.);
#2385=ORIENTED_EDGE('',*,*,#1782,.F.);
#2386=ORIENTED_EDGE('',*,*,#1781,.T.);
#2387=ORIENTED_EDGE('',*,*,#1784,.F.);
#2388=ORIENTED_EDGE('',*,*,#1785,.F.);
#2389=ORIENTED_EDGE('',*,*,#1786,.T.);
#2390=ORIENTED_EDGE('',*,*,#1787,.T.);
#2391=ORIENTED_EDGE('',*,*,#1786,.F.);
#2392=ORIENTED_EDGE('',*,*,#1787,.F.);
#2393=ORIENTED_EDGE('',*,*,#1788,.F.);
#2394=ORIENTED_EDGE('',*,*,#1788,.T.);
#2395=ORIENTED_EDGE('',*,*,#1789,.T.);
#2396=ORIENTED_EDGE('',*,*,#1784,.T.);
#2397=ORIENTED_EDGE('',*,*,#1789,.F.);
#2398=ORIENTED_EDGE('',*,*,#1790,.F.);
#2399=ORIENTED_EDGE('',*,*,#1791,.T.);
#2400=ORIENTED_EDGE('',*,*,#1792,.T.);
#2401=ORIENTED_EDGE('',*,*,#1791,.F.);
#2402=ORIENTED_EDGE('',*,*,#1790,.T.);
#2403=ORIENTED_EDGE('',*,*,#1783,.T.);
#2404=ORIENTED_EDGE('',*,*,#1792,.F.);
#2405=ORIENTED_EDGE('',*,*,#1785,.T.);
#2406=ORIENTED_EDGE('',*,*,#1793,.F.);
#2407=ORIENTED_EDGE('',*,*,#1794,.F.);
#2408=ORIENTED_EDGE('',*,*,#1795,.T.);
#2409=ORIENTED_EDGE('',*,*,#1796,.F.);
#2410=ORIENTED_EDGE('',*,*,#1797,.F.);
#2411=ORIENTED_EDGE('',*,*,#1795,.F.);
#2412=ORIENTED_EDGE('',*,*,#1796,.T.);
#2413=ORIENTED_EDGE('',*,*,#1797,.T.);
#2414=ORIENTED_EDGE('',*,*,#1798,.T.);
#2415=ORIENTED_EDGE('',*,*,#1799,.T.);
#2416=ORIENTED_EDGE('',*,*,#1798,.F.);
#2417=ORIENTED_EDGE('',*,*,#1800,.T.);
#2418=ORIENTED_EDGE('',*,*,#1801,.T.);
#2419=ORIENTED_EDGE('',*,*,#1802,.F.);
#2420=ORIENTED_EDGE('',*,*,#1801,.F.);
#2421=ORIENTED_EDGE('',*,*,#1802,.T.);
#2422=ORIENTED_EDGE('',*,*,#1803,.T.);
#2423=ORIENTED_EDGE('',*,*,#1804,.F.);
#2424=ORIENTED_EDGE('',*,*,#1803,.F.);
#2425=ORIENTED_EDGE('',*,*,#1799,.F.);
#2426=ORIENTED_EDGE('',*,*,#1804,.T.);
#2427=ORIENTED_EDGE('',*,*,#1805,.F.);
#2428=ORIENTED_EDGE('',*,*,#1806,.T.);
#2429=ORIENTED_EDGE('',*,*,#1793,.T.);
#2430=ORIENTED_EDGE('',*,*,#1794,.T.);
#2431=ORIENTED_EDGE('',*,*,#1806,.F.);
#2432=ORIENTED_EDGE('',*,*,#1805,.T.);
#2433=ORIENTED_EDGE('',*,*,#1807,.F.);
#2434=ORIENTED_EDGE('',*,*,#1807,.T.);
#2435=ORIENTED_EDGE('',*,*,#1808,.T.);
#2436=ORIENTED_EDGE('',*,*,#1800,.F.);
#2437=ORIENTED_EDGE('',*,*,#1808,.F.);
#2438=ORIENTED_EDGE('',*,*,#1809,.F.);
#2439=ORIENTED_EDGE('',*,*,#1810,.F.);
#2440=ORIENTED_EDGE('',*,*,#1811,.T.);
#2441=ORIENTED_EDGE('',*,*,#1812,.F.);
#2442=ORIENTED_EDGE('',*,*,#1813,.F.);
#2443=ORIENTED_EDGE('',*,*,#1811,.F.);
#2444=ORIENTED_EDGE('',*,*,#1814,.T.);
#2445=ORIENTED_EDGE('',*,*,#1815,.T.);
#2446=ORIENTED_EDGE('',*,*,#1812,.T.);
#2447=ORIENTED_EDGE('',*,*,#1813,.T.);
#2448=ORIENTED_EDGE('',*,*,#1815,.F.);
#2449=ORIENTED_EDGE('',*,*,#1816,.F.);
#2450=ORIENTED_EDGE('',*,*,#1817,.T.);
#2451=ORIENTED_EDGE('',*,*,#1818,.F.);
#2452=ORIENTED_EDGE('',*,*,#1819,.T.);
#2453=ORIENTED_EDGE('',*,*,#1816,.T.);
#2454=ORIENTED_EDGE('',*,*,#1819,.F.);
#2455=ORIENTED_EDGE('',*,*,#1820,.F.);
#2456=ORIENTED_EDGE('',*,*,#1821,.T.);
#2457=ORIENTED_EDGE('',*,*,#1818,.T.);
#2458=ORIENTED_EDGE('',*,*,#1821,.F.);
#2459=ORIENTED_EDGE('',*,*,#1822,.F.);
#2460=ORIENTED_EDGE('',*,*,#1823,.T.);
#2461=ORIENTED_EDGE('',*,*,#1820,.T.);
#2462=ORIENTED_EDGE('',*,*,#1823,.F.);
#2463=ORIENTED_EDGE('',*,*,#1822,.T.);
#2464=ORIENTED_EDGE('',*,*,#1814,.F.);
#2465=ORIENTED_EDGE('',*,*,#1809,.T.);
#2466=ORIENTED_EDGE('',*,*,#1810,.T.);
#2467=ORIENTED_EDGE('',*,*,#1824,.T.);
#2468=ORIENTED_EDGE('',*,*,#1817,.F.);
#2469=ORIENTED_EDGE('',*,*,#1824,.F.);
#2470=ORIENTED_EDGE('',*,*,#1825,.T.);
#2471=ORIENTED_EDGE('',*,*,#1825,.F.);
#2472=ORIENTED_EDGE('',*,*,#1826,.T.);
#2473=ORIENTED_EDGE('',*,*,#1826,.F.);
#2474=ORIENTED_EDGE('',*,*,#1827,.T.);
#2475=ORIENTED_EDGE('',*,*,#1827,.F.);
#2476=ORIENTED_EDGE('',*,*,#1828,.T.);
#2477=ORIENTED_EDGE('',*,*,#1828,.F.);
#2478=ORIENTED_EDGE('',*,*,#1829,.T.);
#2479=ORIENTED_EDGE('',*,*,#1829,.F.);
#2480=ORIENTED_EDGE('',*,*,#1830,.T.);
#2481=ORIENTED_EDGE('',*,*,#1830,.F.);
#2482=ORIENTED_EDGE('',*,*,#1831,.T.);
#2483=ORIENTED_EDGE('',*,*,#1831,.F.);
#2484=ORIENTED_EDGE('',*,*,#1832,.F.);
#2485=ORIENTED_EDGE('',*,*,#1833,.F.);
#2486=ORIENTED_EDGE('',*,*,#1834,.F.);
#2487=ORIENTED_EDGE('',*,*,#1835,.F.);
#2488=ORIENTED_EDGE('',*,*,#1834,.T.);
#2489=ORIENTED_EDGE('',*,*,#1836,.F.);
#2490=ORIENTED_EDGE('',*,*,#1837,.T.);
#2491=ORIENTED_EDGE('',*,*,#1838,.F.);
#2492=ORIENTED_EDGE('',*,*,#1839,.T.);
#2493=ORIENTED_EDGE('',*,*,#1840,.F.);
#2494=ORIENTED_EDGE('',*,*,#1841,.T.);
#2495=ORIENTED_EDGE('',*,*,#1842,.F.);
#2496=ORIENTED_EDGE('',*,*,#1841,.F.);
#2497=ORIENTED_EDGE('',*,*,#1843,.F.);
#2498=ORIENTED_EDGE('',*,*,#1844,.T.);
#2499=ORIENTED_EDGE('',*,*,#1845,.F.);
#2500=ORIENTED_EDGE('',*,*,#1846,.T.);
#2501=ORIENTED_EDGE('',*,*,#1847,.F.);
#2502=ORIENTED_EDGE('',*,*,#1848,.T.);
#2503=ORIENTED_EDGE('',*,*,#1849,.F.);
#2504=ORIENTED_EDGE('',*,*,#1850,.T.);
#2505=ORIENTED_EDGE('',*,*,#1851,.F.);
#2506=ORIENTED_EDGE('',*,*,#1833,.T.);
#2507=ORIENTED_EDGE('',*,*,#1852,.T.);
#2508=ORIENTED_EDGE('',*,*,#1853,.T.);
#2509=ORIENTED_EDGE('',*,*,#1836,.T.);
#2510=ORIENTED_EDGE('',*,*,#1854,.F.);
#2511=ORIENTED_EDGE('',*,*,#1855,.F.);
#2512=ORIENTED_EDGE('',*,*,#1837,.F.);
#2513=ORIENTED_EDGE('',*,*,#1853,.F.);
#2514=ORIENTED_EDGE('',*,*,#1855,.T.);
#2515=ORIENTED_EDGE('',*,*,#1856,.T.);
#2516=ORIENTED_EDGE('',*,*,#1857,.T.);
#2517=ORIENTED_EDGE('',*,*,#1838,.T.);
#2518=ORIENTED_EDGE('',*,*,#1858,.F.);
#2519=ORIENTED_EDGE('',*,*,#1859,.F.);
#2520=ORIENTED_EDGE('',*,*,#1839,.F.);
#2521=ORIENTED_EDGE('',*,*,#1857,.F.);
#2522=ORIENTED_EDGE('',*,*,#1859,.T.);
#2523=ORIENTED_EDGE('',*,*,#1860,.T.);
#2524=ORIENTED_EDGE('',*,*,#1861,.T.);
#2525=ORIENTED_EDGE('',*,*,#1862,.T.);
#2526=ORIENTED_EDGE('',*,*,#1843,.T.);
#2527=ORIENTED_EDGE('',*,*,#1840,.T.);
#2528=ORIENTED_EDGE('',*,*,#1863,.F.);
#2529=ORIENTED_EDGE('',*,*,#1864,.F.);
#2530=ORIENTED_EDGE('',*,*,#1844,.F.);
#2531=ORIENTED_EDGE('',*,*,#1862,.F.);
#2532=ORIENTED_EDGE('',*,*,#1864,.T.);
#2533=ORIENTED_EDGE('',*,*,#1865,.T.);
#2534=ORIENTED_EDGE('',*,*,#1866,.T.);
#2535=ORIENTED_EDGE('',*,*,#1845,.T.);
#2536=ORIENTED_EDGE('',*,*,#1867,.F.);
#2537=ORIENTED_EDGE('',*,*,#1868,.F.);
#2538=ORIENTED_EDGE('',*,*,#1846,.F.);
#2539=ORIENTED_EDGE('',*,*,#1866,.F.);
#2540=ORIENTED_EDGE('',*,*,#1868,.T.);
#2541=ORIENTED_EDGE('',*,*,#1869,.T.);
#2542=ORIENTED_EDGE('',*,*,#1870,.T.);
#2543=ORIENTED_EDGE('',*,*,#1847,.T.);
#2544=ORIENTED_EDGE('',*,*,#1848,.F.);
#2545=ORIENTED_EDGE('',*,*,#1870,.F.);
#2546=ORIENTED_EDGE('',*,*,#1871,.F.);
#2547=ORIENTED_EDGE('',*,*,#1872,.F.);
#2548=ORIENTED_EDGE('',*,*,#1873,.F.);
#2549=ORIENTED_EDGE('',*,*,#1874,.T.);
#2550=ORIENTED_EDGE('',*,*,#1860,.F.);
#2551=ORIENTED_EDGE('',*,*,#1858,.T.);
#2552=ORIENTED_EDGE('',*,*,#1856,.F.);
#2553=ORIENTED_EDGE('',*,*,#1854,.T.);
#2554=ORIENTED_EDGE('',*,*,#1852,.F.);
#2555=ORIENTED_EDGE('',*,*,#1832,.T.);
#2556=ORIENTED_EDGE('',*,*,#1875,.F.);
#2557=ORIENTED_EDGE('',*,*,#1876,.T.);
#2558=ORIENTED_EDGE('',*,*,#1877,.F.);
#2559=ORIENTED_EDGE('',*,*,#1871,.T.);
#2560=ORIENTED_EDGE('',*,*,#1869,.F.);
#2561=ORIENTED_EDGE('',*,*,#1867,.T.);
#2562=ORIENTED_EDGE('',*,*,#1865,.F.);
#2563=ORIENTED_EDGE('',*,*,#1863,.T.);
#2564=ORIENTED_EDGE('',*,*,#1861,.F.);
#2565=ORIENTED_EDGE('',*,*,#1874,.F.);
#2566=ORIENTED_EDGE('',*,*,#1835,.T.);
#2567=ORIENTED_EDGE('',*,*,#1851,.T.);
#2568=ORIENTED_EDGE('',*,*,#1878,.T.);
#2569=ORIENTED_EDGE('',*,*,#1875,.T.);
#2570=ORIENTED_EDGE('',*,*,#1850,.F.);
#2571=ORIENTED_EDGE('',*,*,#1879,.F.);
#2572=ORIENTED_EDGE('',*,*,#1876,.F.);
#2573=ORIENTED_EDGE('',*,*,#1878,.F.);
#2574=ORIENTED_EDGE('',*,*,#1842,.T.);
#2575=ORIENTED_EDGE('',*,*,#1873,.T.);
#2576=ORIENTED_EDGE('',*,*,#1872,.T.);
#2577=ORIENTED_EDGE('',*,*,#1877,.T.);
#2578=ORIENTED_EDGE('',*,*,#1879,.T.);
#2579=ORIENTED_EDGE('',*,*,#1849,.T.);
#2580=ORIENTED_EDGE('',*,*,#1880,.F.);
#2581=ORIENTED_EDGE('',*,*,#1881,.T.);
#2582=ORIENTED_EDGE('',*,*,#1882,.F.);
#2583=ORIENTED_EDGE('',*,*,#1883,.T.);
#2584=ORIENTED_EDGE('',*,*,#1880,.T.);
#2585=ORIENTED_EDGE('',*,*,#1883,.F.);
#2586=ORIENTED_EDGE('',*,*,#1882,.T.);
#2587=ORIENTED_EDGE('',*,*,#1884,.F.);
#2588=ORIENTED_EDGE('',*,*,#1884,.T.);
#2589=ORIENTED_EDGE('',*,*,#1885,.T.);
#2590=ORIENTED_EDGE('',*,*,#1881,.F.);
#2591=ORIENTED_EDGE('',*,*,#1885,.F.);
#2592=ORIENTED_EDGE('',*,*,#1886,.F.);
#2593=ORIENTED_EDGE('',*,*,#1887,.T.);
#2594=ORIENTED_EDGE('',*,*,#1888,.F.);
#2595=ORIENTED_EDGE('',*,*,#1889,.T.);
#2596=ORIENTED_EDGE('',*,*,#1886,.T.);
#2597=ORIENTED_EDGE('',*,*,#1889,.F.);
#2598=ORIENTED_EDGE('',*,*,#1888,.T.);
#2599=ORIENTED_EDGE('',*,*,#1890,.F.);
#2600=ORIENTED_EDGE('',*,*,#1890,.T.);
#2601=ORIENTED_EDGE('',*,*,#1891,.T.);
#2602=ORIENTED_EDGE('',*,*,#1887,.F.);
#2603=ORIENTED_EDGE('',*,*,#1891,.F.);
#2604=ORIENTED_EDGE('',*,*,#1892,.F.);
#2605=ORIENTED_EDGE('',*,*,#1893,.T.);
#2606=ORIENTED_EDGE('',*,*,#1894,.T.);
#2607=ORIENTED_EDGE('',*,*,#1893,.F.);
#2608=ORIENTED_EDGE('',*,*,#1895,.F.);
#2609=ORIENTED_EDGE('',*,*,#1896,.T.);
#2610=ORIENTED_EDGE('',*,*,#1897,.T.);
#2611=ORIENTED_EDGE('',*,*,#1896,.F.);
#2612=ORIENTED_EDGE('',*,*,#1895,.T.);
#2613=ORIENTED_EDGE('',*,*,#1892,.T.);
#2614=ORIENTED_EDGE('',*,*,#1897,.F.);
#2615=ORIENTED_EDGE('',*,*,#1894,.F.);
#2616=ORIENTED_EDGE('',*,*,#1898,.F.);
#2617=ORIENTED_EDGE('',*,*,#1899,.T.);
#2618=ORIENTED_EDGE('',*,*,#1900,.F.);
#2619=ORIENTED_EDGE('',*,*,#1899,.F.);
#2620=ORIENTED_EDGE('',*,*,#1901,.F.);
#2621=ORIENTED_EDGE('',*,*,#1902,.F.);
#2622=ORIENTED_EDGE('',*,*,#1903,.F.);
#2623=ORIENTED_EDGE('',*,*,#1904,.F.);
#2624=ORIENTED_EDGE('',*,*,#1905,.F.);
#2625=ORIENTED_EDGE('',*,*,#1903,.T.);
#2626=ORIENTED_EDGE('',*,*,#1906,.F.);
#2627=ORIENTED_EDGE('',*,*,#1907,.F.);
#2628=ORIENTED_EDGE('',*,*,#1908,.F.);
#2629=ORIENTED_EDGE('',*,*,#1909,.F.);
#2630=ORIENTED_EDGE('',*,*,#1907,.T.);
#2631=ORIENTED_EDGE('',*,*,#1910,.F.);
#2632=ORIENTED_EDGE('',*,*,#1911,.F.);
#2633=ORIENTED_EDGE('',*,*,#1912,.T.);
#2634=ORIENTED_EDGE('',*,*,#1913,.T.);
#2635=ORIENTED_EDGE('',*,*,#1914,.T.);
#2636=ORIENTED_EDGE('',*,*,#1915,.T.);
#2637=ORIENTED_EDGE('',*,*,#1916,.F.);
#2638=ORIENTED_EDGE('',*,*,#1904,.T.);
#2639=ORIENTED_EDGE('',*,*,#1905,.T.);
#2640=ORIENTED_EDGE('',*,*,#1909,.T.);
#2641=ORIENTED_EDGE('',*,*,#1898,.T.);
#2642=ORIENTED_EDGE('',*,*,#1908,.T.);
#2643=ORIENTED_EDGE('',*,*,#1917,.F.);
#2644=ORIENTED_EDGE('',*,*,#1918,.T.);
#2645=ORIENTED_EDGE('',*,*,#1911,.T.);
#2646=ORIENTED_EDGE('',*,*,#1919,.F.);
#2647=ORIENTED_EDGE('',*,*,#1915,.F.);
#2648=ORIENTED_EDGE('',*,*,#1920,.T.);
#2649=ORIENTED_EDGE('',*,*,#1921,.F.);
#2650=ORIENTED_EDGE('',*,*,#1918,.F.);
#2651=ORIENTED_EDGE('',*,*,#1922,.F.);
#2652=ORIENTED_EDGE('',*,*,#1923,.F.);
#2653=ORIENTED_EDGE('',*,*,#1912,.F.);
#2654=ORIENTED_EDGE('',*,*,#1913,.F.);
#2655=ORIENTED_EDGE('',*,*,#1923,.T.);
#2656=ORIENTED_EDGE('',*,*,#1924,.F.);
#2657=ORIENTED_EDGE('',*,*,#1925,.F.);
#2658=ORIENTED_EDGE('',*,*,#1914,.F.);
#2659=ORIENTED_EDGE('',*,*,#1925,.T.);
#2660=ORIENTED_EDGE('',*,*,#1926,.F.);
#2661=ORIENTED_EDGE('',*,*,#1920,.F.);
#2662=ORIENTED_EDGE('',*,*,#1927,.T.);
#2663=ORIENTED_EDGE('',*,*,#1921,.T.);
#2664=ORIENTED_EDGE('',*,*,#1926,.T.);
#2665=ORIENTED_EDGE('',*,*,#1924,.T.);
#2666=ORIENTED_EDGE('',*,*,#1922,.T.);
#2667=ORIENTED_EDGE('',*,*,#1917,.T.);
#2668=ORIENTED_EDGE('',*,*,#1910,.T.);
#2669=ORIENTED_EDGE('',*,*,#1906,.T.);
#2670=ORIENTED_EDGE('',*,*,#1902,.T.);
#2671=ORIENTED_EDGE('',*,*,#1900,.T.);
#2672=ORIENTED_EDGE('',*,*,#1901,.T.);
#2673=ORIENTED_EDGE('',*,*,#1916,.T.);
#2674=ORIENTED_EDGE('',*,*,#1919,.T.);
#2675=ORIENTED_EDGE('',*,*,#1927,.F.);
#2676=ORIENTED_EDGE('',*,*,#1928,.T.);
#2677=ORIENTED_EDGE('',*,*,#1929,.T.);
#2678=ORIENTED_EDGE('',*,*,#1930,.F.);
#2679=ORIENTED_EDGE('',*,*,#1931,.F.);
#2680=ORIENTED_EDGE('',*,*,#1932,.T.);
#2681=ORIENTED_EDGE('',*,*,#1931,.T.);
#2682=ORIENTED_EDGE('',*,*,#1933,.F.);
#2683=ORIENTED_EDGE('',*,*,#1934,.F.);
#2684=ORIENTED_EDGE('',*,*,#1935,.T.);
#2685=ORIENTED_EDGE('',*,*,#1934,.T.);
#2686=ORIENTED_EDGE('',*,*,#1936,.F.);
#2687=ORIENTED_EDGE('',*,*,#1937,.F.);
#2688=ORIENTED_EDGE('',*,*,#1938,.T.);
#2689=ORIENTED_EDGE('',*,*,#1937,.T.);
#2690=ORIENTED_EDGE('',*,*,#1939,.F.);
#2691=ORIENTED_EDGE('',*,*,#1929,.F.);
#2692=ORIENTED_EDGE('',*,*,#1939,.T.);
#2693=ORIENTED_EDGE('',*,*,#1936,.T.);
#2694=ORIENTED_EDGE('',*,*,#1933,.T.);
#2695=ORIENTED_EDGE('',*,*,#1930,.T.);
#2696=ORIENTED_EDGE('',*,*,#1938,.F.);
#2697=ORIENTED_EDGE('',*,*,#1928,.F.);
#2698=ORIENTED_EDGE('',*,*,#1932,.F.);
#2699=ORIENTED_EDGE('',*,*,#1935,.F.);
#2700=PLANE('',#3203);
#2701=PLANE('',#3204);
#2702=PLANE('',#3205);
#2703=PLANE('',#3206);
#2704=PLANE('',#3207);
#2705=PLANE('',#3208);
#2706=PLANE('',#3209);
#2707=PLANE('',#3211);
#2708=PLANE('',#3212);
#2709=PLANE('',#3218);
#2710=PLANE('',#3219);
#2711=PLANE('',#3220);
#2712=PLANE('',#3221);
#2713=PLANE('',#3222);
#2714=PLANE('',#3223);
#2715=PLANE('',#3224);
#2716=PLANE('',#3231);
#2717=PLANE('',#3232);
#2718=PLANE('',#3233);
#2719=PLANE('',#3234);
#2720=PLANE('',#3235);
#2721=PLANE('',#3236);
#2722=PLANE('',#3237);
#2723=PLANE('',#3238);
#2724=PLANE('',#3239);
#2725=PLANE('',#3240);
#2726=PLANE('',#3241);
#2727=PLANE('',#3242);
#2728=PLANE('',#3255);
#2729=PLANE('',#3256);
#2730=PLANE('',#3257);
#2731=PLANE('',#3258);
#2732=PLANE('',#3259);
#2733=PLANE('',#3260);
#2734=PLANE('',#3265);
#2735=PLANE('',#3266);
#2736=PLANE('',#3271);
#2737=PLANE('',#3274);
#2738=PLANE('',#3282);
#2739=PLANE('',#3283);
#2740=PLANE('',#3291);
#2741=PLANE('',#3292);
#2742=PLANE('',#3294);
#2743=PLANE('',#3295);
#2744=PLANE('',#3296);
#2745=PLANE('',#3297);
#2746=PLANE('',#3298);
#2747=PLANE('',#3299);
#2748=PLANE('',#3300);
#2749=PLANE('',#3301);
#2750=PLANE('',#3302);
#2751=PLANE('',#3304);
#2752=PLANE('',#3312);
#2753=PLANE('',#3324);
#2754=PLANE('',#3325);
#2755=PLANE('',#3332);
#2756=PLANE('',#3335);
#2757=PLANE('',#3336);
#2758=PLANE('',#3337);
#2759=PLANE('',#3338);
#2760=PLANE('',#3339);
#2761=PLANE('',#3340);
#2762=PLANE('',#3341);
#2763=PLANE('',#3342);
#2764=PLANE('',#3348);
#2765=PLANE('',#3349);
#2766=PLANE('',#3350);
#2767=PLANE('',#3354);
#2768=PLANE('',#3355);
#2769=PLANE('',#3356);
#2770=PLANE('',#3357);
#2771=PLANE('',#3358);
#2772=PLANE('',#3374);
#2773=PLANE('',#3379);
#2774=PLANE('',#3385);
#2775=PLANE('',#3386);
#2776=PLANE('',#3402);
#2777=PLANE('',#3405);
#2778=PLANE('',#3417);
#2779=PLANE('',#3426);
#2780=PLANE('',#3457);
#2781=PLANE('',#3462);
#2782=PLANE('',#3467);
#2783=PLANE('',#3473);
#2784=PLANE('',#3478);
#2785=PLANE('',#3487);
#2786=PLANE('',#3491);
#2787=PLANE('',#3492);
#2788=PLANE('',#3494);
#2789=PLANE('',#3499);
#2790=PLANE('',#3502);
#2791=PLANE('',#3507);
#2792=PLANE('',#3522);
#2793=PLANE('',#3523);
#2794=PLANE('',#3534);
#2795=PLANE('',#3535);
#2796=PLANE('',#3536);
#2797=PLANE('',#3537);
#2798=PLANE('',#3542);
#2799=PLANE('',#3543);
#2800=PLANE('',#3544);
#2801=PLANE('',#3545);
#2802=PLANE('',#3546);
#2803=PLANE('',#3550);
#2804=PLANE('',#3551);
#2805=PLANE('',#3552);
#2806=PLANE('',#3553);
#2807=PLANE('',#3554);
#2808=PLANE('',#3555);
#2809=ADVANCED_FACE('',(#476),#2700,.F.);
#2810=ADVANCED_FACE('',(#477),#2701,.F.);
#2811=ADVANCED_FACE('',(#478),#2702,.T.);
#2812=ADVANCED_FACE('',(#479),#2703,.T.);
#2813=ADVANCED_FACE('',(#480),#2704,.F.);
#2814=ADVANCED_FACE('',(#481),#2705,.F.);
#2815=ADVANCED_FACE('',(#482,#295),#2706,.F.);
#2816=ADVANCED_FACE('',(#483),#2707,.T.);
#2817=ADVANCED_FACE('',(#484),#2708,.T.);
#2818=ADVANCED_FACE('',(#485),#253,.F.);
#2819=ADVANCED_FACE('',(#486),#254,.F.);
#2820=ADVANCED_FACE('',(#487,#296),#2709,.T.);
#2821=ADVANCED_FACE('',(#488),#2710,.T.);
#2822=ADVANCED_FACE('',(#489),#2711,.T.);
#2823=ADVANCED_FACE('',(#490,#297),#2712,.T.);
#2824=ADVANCED_FACE('',(#491),#2713,.T.);
#2825=ADVANCED_FACE('',(#492),#2714,.T.);
#2826=ADVANCED_FACE('',(#493,#298),#2715,.F.);
#2827=ADVANCED_FACE('',(#494),#255,.F.);
#2828=ADVANCED_FACE('',(#495),#256,.F.);
#2829=ADVANCED_FACE('',(#496),#2716,.F.);
#2830=ADVANCED_FACE('',(#497),#2717,.T.);
#2831=ADVANCED_FACE('',(#498),#2718,.F.);
#2832=ADVANCED_FACE('',(#499),#2719,.T.);
#2833=ADVANCED_FACE('',(#500),#2720,.T.);
#2834=ADVANCED_FACE('',(#501),#2721,.T.);
#2835=ADVANCED_FACE('',(#502),#2722,.T.);
#2836=ADVANCED_FACE('',(#503),#2723,.T.);
#2837=ADVANCED_FACE('',(#504),#2724,.T.);
#2838=ADVANCED_FACE('',(#505),#2725,.T.);
#2839=ADVANCED_FACE('',(#506),#2726,.T.);
#2840=ADVANCED_FACE('',(#507),#2727,.T.);
#2841=ADVANCED_FACE('',(#508),#257,.F.);
#2842=ADVANCED_FACE('',(#509),#258,.F.);
#2843=ADVANCED_FACE('',(#510),#259,.F.);
#2844=ADVANCED_FACE('',(#511),#260,.F.);
#2845=ADVANCED_FACE('',(#512),#2728,.T.);
#2846=ADVANCED_FACE('',(#513),#2729,.T.);
#2847=ADVANCED_FACE('',(#514),#2730,.T.);
#2848=ADVANCED_FACE('',(#515),#2731,.T.);
#2849=ADVANCED_FACE('',(#516,#299,#300,#301,#302,#303),#2732,.T.);
#2850=ADVANCED_FACE('',(#517,#304,#305,#306,#307,#308,#309,#310),#2733,
 .F.);
#2851=ADVANCED_FACE('',(#518),#261,.F.);
#2852=ADVANCED_FACE('',(#519),#2734,.T.);
#2853=ADVANCED_FACE('',(#520,#311),#2735,.T.);
#2854=ADVANCED_FACE('',(#521),#262,.T.);
#2855=ADVANCED_FACE('',(#522),#2736,.F.);
#2856=ADVANCED_FACE('',(#523),#263,.T.);
#2857=ADVANCED_FACE('',(#524,#312),#2737,.T.);
#2858=ADVANCED_FACE('',(#525),#264,.F.);
#2859=ADVANCED_FACE('',(#526),#265,.T.);
#2860=ADVANCED_FACE('',(#527,#313),#2738,.T.);
#2861=ADVANCED_FACE('',(#528,#314),#2739,.F.);
#2862=ADVANCED_FACE('',(#529),#266,.F.);
#2863=ADVANCED_FACE('',(#530),#267,.T.);
#2864=ADVANCED_FACE('',(#531,#315),#2740,.T.);
#2865=ADVANCED_FACE('',(#532,#316),#2741,.F.);
#2866=ADVANCED_FACE('',(#533),#2742,.F.);
#2867=ADVANCED_FACE('',(#534),#2743,.F.);
#2868=ADVANCED_FACE('',(#535),#2744,.F.);
#2869=ADVANCED_FACE('',(#536),#2745,.F.);
#2870=ADVANCED_FACE('',(#537),#2746,.F.);
#2871=ADVANCED_FACE('',(#538),#2747,.F.);
#2872=ADVANCED_FACE('',(#539),#2748,.F.);
#2873=ADVANCED_FACE('',(#540),#2749,.F.);
#2874=ADVANCED_FACE('',(#541),#2750,.F.);
#2875=ADVANCED_FACE('',(#542),#2751,.T.);
#2876=ADVANCED_FACE('',(#543),#159,.T.);
#2877=ADVANCED_FACE('',(#544),#268,.T.);
#2878=ADVANCED_FACE('',(#545),#160,.T.);
#2879=ADVANCED_FACE('',(#546,#317),#2752,.T.);
#2880=ADVANCED_FACE('',(#547),#161,.T.);
#2881=ADVANCED_FACE('',(#548),#269,.T.);
#2882=ADVANCED_FACE('',(#549),#270,.F.);
#2883=ADVANCED_FACE('',(#550),#271,.T.);
#2884=ADVANCED_FACE('',(#551,#318),#2753,.T.);
#2885=ADVANCED_FACE('',(#552,#319),#2754,.F.);
#2886=ADVANCED_FACE('',(#553),#272,.T.);
#2887=ADVANCED_FACE('',(#554),#162,.T.);
#2888=ADVANCED_FACE('',(#555),#2755,.T.);
#2889=ADVANCED_FACE('',(#556),#163,.T.);
#2890=ADVANCED_FACE('',(#557),#2756,.T.);
#2891=ADVANCED_FACE('',(#558),#2757,.T.);
#2892=ADVANCED_FACE('',(#559),#2758,.T.);
#2893=ADVANCED_FACE('',(#560),#2759,.T.);
#2894=ADVANCED_FACE('',(#561),#2760,.T.);
#2895=ADVANCED_FACE('',(#562),#2761,.T.);
#2896=ADVANCED_FACE('',(#563),#2762,.T.);
#2897=ADVANCED_FACE('',(#564,#320),#2763,.F.);
#2898=ADVANCED_FACE('',(#565),#164,.T.);
#2899=ADVANCED_FACE('',(#566),#165,.T.);
#2900=ADVANCED_FACE('',(#567),#2764,.T.);
#2901=ADVANCED_FACE('',(#568),#2765,.T.);
#2902=ADVANCED_FACE('',(#569),#2766,.T.);
#2903=ADVANCED_FACE('',(#570),#273,.F.);
#2904=ADVANCED_FACE('',(#571),#2767,.T.);
#2905=ADVANCED_FACE('',(#572),#2768,.T.);
#2906=ADVANCED_FACE('',(#573),#2769,.T.);
#2907=ADVANCED_FACE('',(#574,#321),#2770,.T.);
#2908=ADVANCED_FACE('',(#575,#322),#2771,.F.);
#2909=ADVANCED_FACE('',(#576),#274,.F.);
#2910=ADVANCED_FACE('',(#577,#323),#2772,.T.);
#2911=ADVANCED_FACE('',(#578),#275,.F.);
#2912=ADVANCED_FACE('',(#579,#324),#2773,.F.);
#2913=ADVANCED_FACE('',(#580),#276,.F.);
#2914=ADVANCED_FACE('',(#581),#277,.T.);
#2915=ADVANCED_FACE('',(#582,#325),#2774,.T.);
#2916=ADVANCED_FACE('',(#583,#326),#2775,.F.);
#2917=ADVANCED_FACE('',(#584),#39,.F.);
#2918=ADVANCED_FACE('',(#585),#278,.T.);
#2919=ADVANCED_FACE('',(#586),#279,.F.);
#2920=ADVANCED_FACE('',(#587),#166,.F.);
#2921=ADVANCED_FACE('',(#588,#327),#2776,.T.);
#2922=ADVANCED_FACE('',(#589),#280,.T.);
#2923=ADVANCED_FACE('',(#590,#328),#2777,.T.);
#2924=ADVANCED_FACE('',(#591),#167,.F.);
#2925=ADVANCED_FACE('',(#592),#40,.F.);
#2926=ADVANCED_FACE('',(#593),#281,.F.);
#2927=ADVANCED_FACE('',(#594,#329),#2778,.T.);
#2928=ADVANCED_FACE('',(#595),#168,.T.);
#2929=ADVANCED_FACE('',(#596),#282,.T.);
#2930=ADVANCED_FACE('',(#597),#169,.T.);
#2931=ADVANCED_FACE('',(#598,#330),#2779,.T.);
#2932=ADVANCED_FACE('',(#599),#283,.F.);
#2933=ADVANCED_FACE('',(#600),#25,.T.);
#2934=ADVANCED_FACE('',(#601),#26,.T.);
#2935=ADVANCED_FACE('',(#602),#27,.T.);
#2936=ADVANCED_FACE('',(#603),#28,.T.);
#2937=ADVANCED_FACE('',(#604),#29,.T.);
#2938=ADVANCED_FACE('',(#605),#30,.T.);
#2939=ADVANCED_FACE('',(#606),#31,.T.);
#2940=ADVANCED_FACE('',(#607),#32,.F.);
#2941=ADVANCED_FACE('',(#608),#284,.T.);
#2942=ADVANCED_FACE('',(#609),#2780,.T.);
#2943=ADVANCED_FACE('',(#610),#33,.F.);
#2944=ADVANCED_FACE('',(#611),#2781,.T.);
#2945=ADVANCED_FACE('',(#612),#34,.F.);
#2946=ADVANCED_FACE('',(#613),#2782,.T.);
#2947=ADVANCED_FACE('',(#614),#35,.F.);
#2948=ADVANCED_FACE('',(#615),#2783,.T.);
#2949=ADVANCED_FACE('',(#616),#36,.F.);
#2950=ADVANCED_FACE('',(#617),#2784,.T.);
#2951=ADVANCED_FACE('',(#618),#37,.F.);
#2952=ADVANCED_FACE('',(#619),#285,.F.);
#2953=ADVANCED_FACE('',(#620),#2785,.T.);
#2954=ADVANCED_FACE('',(#621),#38,.F.);
#2955=ADVANCED_FACE('',(#622,#331),#2786,.T.);
#2956=ADVANCED_FACE('',(#623),#2787,.T.);
#2957=ADVANCED_FACE('',(#624,#332),#2788,.T.);
#2958=ADVANCED_FACE('',(#625),#286,.T.);
#2959=ADVANCED_FACE('',(#626,#333),#2789,.T.);
#2960=ADVANCED_FACE('',(#627),#287,.F.);
#2961=ADVANCED_FACE('',(#628,#334),#2790,.T.);
#2962=ADVANCED_FACE('',(#629),#288,.T.);
#2963=ADVANCED_FACE('',(#630,#335),#2791,.T.);
#2964=ADVANCED_FACE('',(#631),#289,.F.);
#2965=ADVANCED_FACE('',(#632),#290,.F.);
#2966=ADVANCED_FACE('',(#633),#291,.T.);
#2967=ADVANCED_FACE('',(#634,#336),#2792,.T.);
#2968=ADVANCED_FACE('',(#635,#337),#2793,.F.);
#2969=ADVANCED_FACE('',(#636),#292,.F.);
#2970=ADVANCED_FACE('',(#637),#2794,.T.);
#2971=ADVANCED_FACE('',(#638),#2795,.T.);
#2972=ADVANCED_FACE('',(#639),#2796,.T.);
#2973=ADVANCED_FACE('',(#640,#338),#2797,.F.);
#2974=ADVANCED_FACE('',(#641),#293,.T.);
#2975=ADVANCED_FACE('',(#642),#2798,.T.);
#2976=ADVANCED_FACE('',(#643),#2799,.T.);
#2977=ADVANCED_FACE('',(#644),#2800,.T.);
#2978=ADVANCED_FACE('',(#645),#2801,.T.);
#2979=ADVANCED_FACE('',(#646,#339),#2802,.T.);
#2980=ADVANCED_FACE('',(#647),#294,.T.);
#2981=ADVANCED_FACE('',(#648),#2803,.T.);
#2982=ADVANCED_FACE('',(#649),#2804,.T.);
#2983=ADVANCED_FACE('',(#650),#2805,.T.);
#2984=ADVANCED_FACE('',(#651),#2806,.T.);
#2985=ADVANCED_FACE('',(#652),#2807,.T.);
#2986=ADVANCED_FACE('',(#653),#2808,.F.);
#2987=CLOSED_SHELL('',(#2809,#2810,#2811,#2812,#2813,#2814,#2815,#2816,
#2817,#2818,#2819,#2820,#2821,#2822,#2823,#2824,#2825,#2826,#2827,#2828,
#2829,#2830,#2831,#2832,#2833,#2834,#2835,#2836,#2837,#2838,#2839,#2840,
#2841,#2842,#2843,#2844,#2845,#2846,#2847,#2848,#2849,#2850));
#2988=CLOSED_SHELL('',(#2851,#2852,#2853,#2854,#2855,#2856,#2857));
#2989=CLOSED_SHELL('',(#2858,#2859,#2860,#2861));
#2990=CLOSED_SHELL('',(#2862,#2863,#2864,#2865));
#2991=CLOSED_SHELL('',(#2866,#2867,#2868,#2869,#2870,#2871,#2872,#2873));
#2992=CLOSED_SHELL('',(#2874,#2875,#2876,#2877,#2878,#2879,#2880,#2881));
#2993=CLOSED_SHELL('',(#2882,#2883,#2884,#2885));
#2994=CLOSED_SHELL('',(#2886,#2887,#2888,#2889,#2890,#2891,#2892,#2893,
#2894,#2895,#2896,#2897));
#2995=CLOSED_SHELL('',(#2898,#2899,#2900,#2901,#2902,#2903,#2904,#2905,
#2906,#2907,#2908));
#2996=CLOSED_SHELL('',(#2909,#2910,#2911,#2912,#2913,#2914,#2915,#2916));
#2997=CLOSED_SHELL('',(#2917,#2918,#2919,#2920,#2921,#2922,#2923,#2924));
#2998=CLOSED_SHELL('',(#2925,#2926,#2927,#2928,#2929,#2930,#2931,#2932));
#2999=CLOSED_SHELL('',(#2933));
#3000=CLOSED_SHELL('',(#2934));
#3001=CLOSED_SHELL('',(#2935));
#3002=CLOSED_SHELL('',(#2936));
#3003=CLOSED_SHELL('',(#2937));
#3004=CLOSED_SHELL('',(#2938));
#3005=CLOSED_SHELL('',(#2939));
#3006=CLOSED_SHELL('',(#2940,#2941,#2942,#2943,#2944,#2945,#2946,#2947,
#2948,#2949,#2950,#2951,#2952,#2953,#2954,#2955,#2956));
#3007=CLOSED_SHELL('',(#2957,#2958,#2959,#2960));
#3008=CLOSED_SHELL('',(#2961,#2962,#2963,#2964));
#3009=CLOSED_SHELL('',(#2965,#2966,#2967,#2968));
#3010=CLOSED_SHELL('',(#2969,#2970,#2971,#2972,#2973,#2974,#2975,#2976,
#2977,#2978,#2979,#2980));
#3011=CLOSED_SHELL('',(#2981,#2982,#2983,#2984,#2985,#2986));
#3012=DERIVED_UNIT_ELEMENT(#3046,1.);
#3013=DERIVED_UNIT_ELEMENT(#5736,-3.);
#3014=DERIVED_UNIT_ELEMENT(#3046,1.);
#3015=DERIVED_UNIT_ELEMENT(#5736,-3.);
#3016=DERIVED_UNIT_ELEMENT(#3046,1.);
#3017=DERIVED_UNIT_ELEMENT(#5736,-3.);
#3018=DERIVED_UNIT_ELEMENT(#3046,1.);
#3019=DERIVED_UNIT_ELEMENT(#5736,-3.);
#3020=DERIVED_UNIT_ELEMENT(#3046,1.);
#3021=DERIVED_UNIT_ELEMENT(#5736,-3.);
#3022=DERIVED_UNIT_ELEMENT(#3046,1.);
#3023=DERIVED_UNIT_ELEMENT(#5736,-3.);
#3024=DERIVED_UNIT_ELEMENT(#3046,1.);
#3025=DERIVED_UNIT_ELEMENT(#5736,-3.);
#3026=DERIVED_UNIT_ELEMENT(#3046,1.);
#3027=DERIVED_UNIT_ELEMENT(#5736,-3.);
#3028=DERIVED_UNIT_ELEMENT(#3046,1.);
#3029=DERIVED_UNIT_ELEMENT(#5736,-3.);
#3030=DERIVED_UNIT_ELEMENT(#3046,1.);
#3031=DERIVED_UNIT_ELEMENT(#5736,-3.);
#3032=DERIVED_UNIT_ELEMENT(#3046,1.);
#3033=DERIVED_UNIT_ELEMENT(#5736,-3.);
#3034=DERIVED_UNIT_ELEMENT(#3046,1.);
#3035=DERIVED_UNIT_ELEMENT(#5736,-3.);
#3036=DERIVED_UNIT_ELEMENT(#3046,1.);
#3037=DERIVED_UNIT_ELEMENT(#5736,-3.);
#3038=DERIVED_UNIT_ELEMENT(#3046,1.);
#3039=DERIVED_UNIT_ELEMENT(#5736,-3.);
#3040=DERIVED_UNIT_ELEMENT(#3046,1.);
#3041=DERIVED_UNIT_ELEMENT(#5736,-3.);
#3042=DERIVED_UNIT_ELEMENT(#3046,1.);
#3043=DERIVED_UNIT_ELEMENT(#5736,-3.);
#3044=DERIVED_UNIT_ELEMENT(#3046,1.);
#3045=DERIVED_UNIT_ELEMENT(#5736,-3.);
#3046=(
MASS_UNIT()
NAMED_UNIT(*)
SI_UNIT(.KILO.,.GRAM.)
);
#3047=DERIVED_UNIT((#3012,#3013));
#3048=DERIVED_UNIT((#3014,#3015));
#3049=DERIVED_UNIT((#3016,#3017));
#3050=DERIVED_UNIT((#3018,#3019));
#3051=DERIVED_UNIT((#3020,#3021));
#3052=DERIVED_UNIT((#3022,#3023));
#3053=DERIVED_UNIT((#3024,#3025));
#3054=DERIVED_UNIT((#3026,#3027));
#3055=DERIVED_UNIT((#3028,#3029));
#3056=DERIVED_UNIT((#3030,#3031));
#3057=DERIVED_UNIT((#3032,#3033));
#3058=DERIVED_UNIT((#3034,#3035));
#3059=DERIVED_UNIT((#3036,#3037));
#3060=DERIVED_UNIT((#3038,#3039));
#3061=DERIVED_UNIT((#3040,#3041));
#3062=DERIVED_UNIT((#3042,#3043));
#3063=DERIVED_UNIT((#3044,#3045));
#3064=MEASURE_REPRESENTATION_ITEM('density measure',
POSITIVE_RATIO_MEASURE(7850.),#3047);
#3065=MEASURE_REPRESENTATION_ITEM('density measure',
POSITIVE_RATIO_MEASURE(7850.),#3048);
#3066=MEASURE_REPRESENTATION_ITEM('density measure',
POSITIVE_RATIO_MEASURE(7850.),#3049);
#3067=MEASURE_REPRESENTATION_ITEM('density measure',
POSITIVE_RATIO_MEASURE(7850.),#3050);
#3068=MEASURE_REPRESENTATION_ITEM('density measure',
POSITIVE_RATIO_MEASURE(7850.),#3051);
#3069=MEASURE_REPRESENTATION_ITEM('density measure',
POSITIVE_RATIO_MEASURE(7850.),#3052);
#3070=MEASURE_REPRESENTATION_ITEM('density measure',
POSITIVE_RATIO_MEASURE(7850.),#3053);
#3071=MEASURE_REPRESENTATION_ITEM('density measure',
POSITIVE_RATIO_MEASURE(7850.),#3054);
#3072=MEASURE_REPRESENTATION_ITEM('density measure',
POSITIVE_RATIO_MEASURE(7850.),#3055);
#3073=MEASURE_REPRESENTATION_ITEM('density measure',
POSITIVE_RATIO_MEASURE(7850.),#3056);
#3074=MEASURE_REPRESENTATION_ITEM('density measure',
POSITIVE_RATIO_MEASURE(7850.),#3057);
#3075=MEASURE_REPRESENTATION_ITEM('density measure',
POSITIVE_RATIO_MEASURE(7850.),#3058);
#3076=MEASURE_REPRESENTATION_ITEM('density measure',
POSITIVE_RATIO_MEASURE(7850.),#3059);
#3077=MEASURE_REPRESENTATION_ITEM('density measure',
POSITIVE_RATIO_MEASURE(7850.),#3060);
#3078=MEASURE_REPRESENTATION_ITEM('density measure',
POSITIVE_RATIO_MEASURE(7850.),#3061);
#3079=MEASURE_REPRESENTATION_ITEM('density measure',
POSITIVE_RATIO_MEASURE(7850.),#3062);
#3080=MEASURE_REPRESENTATION_ITEM('density measure',
POSITIVE_RATIO_MEASURE(7850.),#3063);
#3081=PROPERTY_DEFINITION_REPRESENTATION(#3166,#3115);
#3082=PROPERTY_DEFINITION_REPRESENTATION(#3167,#3116);
#3083=PROPERTY_DEFINITION_REPRESENTATION(#3168,#3117);
#3084=PROPERTY_DEFINITION_REPRESENTATION(#3169,#3118);
#3085=PROPERTY_DEFINITION_REPRESENTATION(#3170,#3119);
#3086=PROPERTY_DEFINITION_REPRESENTATION(#3171,#3120);
#3087=PROPERTY_DEFINITION_REPRESENTATION(#3172,#3121);
#3088=PROPERTY_DEFINITION_REPRESENTATION(#3173,#3122);
#3089=PROPERTY_DEFINITION_REPRESENTATION(#3174,#3123);
#3090=PROPERTY_DEFINITION_REPRESENTATION(#3175,#3124);
#3091=PROPERTY_DEFINITION_REPRESENTATION(#3176,#3125);
#3092=PROPERTY_DEFINITION_REPRESENTATION(#3177,#3126);
#3093=PROPERTY_DEFINITION_REPRESENTATION(#3178,#3127);
#3094=PROPERTY_DEFINITION_REPRESENTATION(#3179,#3128);
#3095=PROPERTY_DEFINITION_REPRESENTATION(#3180,#3129);
#3096=PROPERTY_DEFINITION_REPRESENTATION(#3181,#3130);
#3097=PROPERTY_DEFINITION_REPRESENTATION(#3182,#3131);
#3098=PROPERTY_DEFINITION_REPRESENTATION(#3183,#3132);
#3099=PROPERTY_DEFINITION_REPRESENTATION(#3184,#3133);
#3100=PROPERTY_DEFINITION_REPRESENTATION(#3185,#3134);
#3101=PROPERTY_DEFINITION_REPRESENTATION(#3186,#3135);
#3102=PROPERTY_DEFINITION_REPRESENTATION(#3187,#3136);
#3103=PROPERTY_DEFINITION_REPRESENTATION(#3188,#3137);
#3104=PROPERTY_DEFINITION_REPRESENTATION(#3189,#3138);
#3105=PROPERTY_DEFINITION_REPRESENTATION(#3190,#3139);
#3106=PROPERTY_DEFINITION_REPRESENTATION(#3191,#3140);
#3107=PROPERTY_DEFINITION_REPRESENTATION(#3192,#3141);
#3108=PROPERTY_DEFINITION_REPRESENTATION(#3193,#3142);
#3109=PROPERTY_DEFINITION_REPRESENTATION(#3194,#3143);
#3110=PROPERTY_DEFINITION_REPRESENTATION(#3195,#3144);
#3111=PROPERTY_DEFINITION_REPRESENTATION(#3196,#3145);
#3112=PROPERTY_DEFINITION_REPRESENTATION(#3197,#3146);
#3113=PROPERTY_DEFINITION_REPRESENTATION(#3198,#3147);
#3114=PROPERTY_DEFINITION_REPRESENTATION(#3199,#3148);
#3115=REPRESENTATION('material name',(#3149),#5714);
#3116=REPRESENTATION('density',(#3064),#5714);
#3117=REPRESENTATION('material name',(#3150),#5715);
#3118=REPRESENTATION('density',(#3065),#5715);
#3119=REPRESENTATION('material name',(#3151),#5716);
#3120=REPRESENTATION('density',(#3066),#5716);
#3121=REPRESENTATION('material name',(#3152),#5717);
#3122=REPRESENTATION('density',(#3067),#5717);
#3123=REPRESENTATION('material name',(#3153),#5718);
#3124=REPRESENTATION('density',(#3068),#5718);
#3125=REPRESENTATION('material name',(#3154),#5719);
#3126=REPRESENTATION('density',(#3069),#5719);
#3127=REPRESENTATION('material name',(#3155),#5720);
#3128=REPRESENTATION('density',(#3070),#5720);
#3129=REPRESENTATION('material name',(#3156),#5721);
#3130=REPRESENTATION('density',(#3071),#5721);
#3131=REPRESENTATION('material name',(#3157),#5723);
#3132=REPRESENTATION('density',(#3072),#5723);
#3133=REPRESENTATION('material name',(#3158),#5725);
#3134=REPRESENTATION('density',(#3073),#5725);
#3135=REPRESENTATION('material name',(#3159),#5726);
#3136=REPRESENTATION('density',(#3074),#5726);
#3137=REPRESENTATION('material name',(#3160),#5727);
#3138=REPRESENTATION('density',(#3075),#5727);
#3139=REPRESENTATION('material name',(#3161),#5728);
#3140=REPRESENTATION('density',(#3076),#5728);
#3141=REPRESENTATION('material name',(#3162),#5729);
#3142=REPRESENTATION('density',(#3077),#5729);
#3143=REPRESENTATION('material name',(#3163),#5730);
#3144=REPRESENTATION('density',(#3078),#5730);
#3145=REPRESENTATION('material name',(#3164),#5732);
#3146=REPRESENTATION('density',(#3079),#5732);
#3147=REPRESENTATION('material name',(#3165),#5733);
#3148=REPRESENTATION('density',(#3080),#5733);
#3149=DESCRIPTIVE_REPRESENTATION_ITEM('Steel','Steel');
#3150=DESCRIPTIVE_REPRESENTATION_ITEM('Steel','Steel');
#3151=DESCRIPTIVE_REPRESENTATION_ITEM('Steel','Steel');
#3152=DESCRIPTIVE_REPRESENTATION_ITEM('Steel','Steel');
#3153=DESCRIPTIVE_REPRESENTATION_ITEM('Steel','Steel');
#3154=DESCRIPTIVE_REPRESENTATION_ITEM('Steel','Steel');
#3155=DESCRIPTIVE_REPRESENTATION_ITEM('Steel','Steel');
#3156=DESCRIPTIVE_REPRESENTATION_ITEM('Steel','Steel');
#3157=DESCRIPTIVE_REPRESENTATION_ITEM('Steel','Steel');
#3158=DESCRIPTIVE_REPRESENTATION_ITEM('Steel','Steel');
#3159=DESCRIPTIVE_REPRESENTATION_ITEM('Steel','Steel');
#3160=DESCRIPTIVE_REPRESENTATION_ITEM('Steel','Steel');
#3161=DESCRIPTIVE_REPRESENTATION_ITEM('Steel','Steel');
#3162=DESCRIPTIVE_REPRESENTATION_ITEM('Steel','Steel');
#3163=DESCRIPTIVE_REPRESENTATION_ITEM('Steel','Steel');
#3164=DESCRIPTIVE_REPRESENTATION_ITEM('Steel','Steel');
#3165=DESCRIPTIVE_REPRESENTATION_ITEM('Steel','Steel');
#3166=PROPERTY_DEFINITION('material property','material name',#5833);
#3167=PROPERTY_DEFINITION('material property','density of part',#5833);
#3168=PROPERTY_DEFINITION('material property','material name',#5834);
#3169=PROPERTY_DEFINITION('material property','density of part',#5834);
#3170=PROPERTY_DEFINITION('material property','material name',#5835);
#3171=PROPERTY_DEFINITION('material property','density of part',#5835);
#3172=PROPERTY_DEFINITION('material property','material name',#5836);
#3173=PROPERTY_DEFINITION('material property','density of part',#5836);
#3174=PROPERTY_DEFINITION('material property','material name',#5837);
#3175=PROPERTY_DEFINITION('material property','density of part',#5837);
#3176=PROPERTY_DEFINITION('material property','material name',#5838);
#3177=PROPERTY_DEFINITION('material property','density of part',#5838);
#3178=PROPERTY_DEFINITION('material property','material name',#5839);
#3179=PROPERTY_DEFINITION('material property','density of part',#5839);
#3180=PROPERTY_DEFINITION('material property','material name',#5840);
#3181=PROPERTY_DEFINITION('material property','density of part',#5840);
#3182=PROPERTY_DEFINITION('material property','material name',#5842);
#3183=PROPERTY_DEFINITION('material property','density of part',#5842);
#3184=PROPERTY_DEFINITION('material property','material name',#5844);
#3185=PROPERTY_DEFINITION('material property','density of part',#5844);
#3186=PROPERTY_DEFINITION('material property','material name',#5845);
#3187=PROPERTY_DEFINITION('material property','density of part',#5845);
#3188=PROPERTY_DEFINITION('material property','material name',#5846);
#3189=PROPERTY_DEFINITION('material property','density of part',#5846);
#3190=PROPERTY_DEFINITION('material property','material name',#5847);
#3191=PROPERTY_DEFINITION('material property','density of part',#5847);
#3192=PROPERTY_DEFINITION('material property','material name',#5848);
#3193=PROPERTY_DEFINITION('material property','density of part',#5848);
#3194=PROPERTY_DEFINITION('material property','material name',#5849);
#3195=PROPERTY_DEFINITION('material property','density of part',#5849);
#3196=PROPERTY_DEFINITION('material property','material name',#5851);
#3197=PROPERTY_DEFINITION('material property','density of part',#5851);
#3198=PROPERTY_DEFINITION('material property','material name',#5852);
#3199=PROPERTY_DEFINITION('material property','density of part',#5852);
#3200=AXIS2_PLACEMENT_3D('',#4495,#3561,#3562);
#3201=AXIS2_PLACEMENT_3D('',#4496,#3563,#3564);
#3202=AXIS2_PLACEMENT_3D('',#4497,#3565,#3566);
#3203=AXIS2_PLACEMENT_3D('',#4498,#3567,#3568);
#3204=AXIS2_PLACEMENT_3D('',#4507,#3573,#3574);
#3205=AXIS2_PLACEMENT_3D('',#4521,#3582,#3583);
#3206=AXIS2_PLACEMENT_3D('',#4527,#3587,#3588);
#3207=AXIS2_PLACEMENT_3D('',#4536,#3593,#3594);
#3208=AXIS2_PLACEMENT_3D('',#4547,#3601,#3602);
#3209=AXIS2_PLACEMENT_3D('',#4550,#3605,#3606);
#3210=AXIS2_PLACEMENT_3D('',#4557,#3610,#3611);
#3211=AXIS2_PLACEMENT_3D('',#4558,#3612,#3613);
#3212=AXIS2_PLACEMENT_3D('',#4564,#3617,#3618);
#3213=AXIS2_PLACEMENT_3D('',#4572,#3623,#3624);
#3214=AXIS2_PLACEMENT_3D('',#4574,#3625,#3626);
#3215=AXIS2_PLACEMENT_3D('',#4577,#3628,#3629);
#3216=AXIS2_PLACEMENT_3D('',#4578,#3630,#3631);
#3217=AXIS2_PLACEMENT_3D('',#4581,#3633,#3634);
#3218=AXIS2_PLACEMENT_3D('',#4582,#3635,#3636);
#3219=AXIS2_PLACEMENT_3D('',#4588,#3640,#3641);
#3220=AXIS2_PLACEMENT_3D('',#4591,#3644,#3645);
#3221=AXIS2_PLACEMENT_3D('',#4592,#3646,#3647);
#3222=AXIS2_PLACEMENT_3D('',#4596,#3650,#3651);
#3223=AXIS2_PLACEMENT_3D('',#4602,#3655,#3656);
#3224=AXIS2_PLACEMENT_3D('',#4604,#3658,#3659);
#3225=AXIS2_PLACEMENT_3D('',#4606,#3661,#3662);
#3226=AXIS2_PLACEMENT_3D('',#4609,#3663,#3664);
#3227=AXIS2_PLACEMENT_3D('',#4613,#3666,#3667);
#3228=AXIS2_PLACEMENT_3D('',#4615,#3669,#3670);
#3229=AXIS2_PLACEMENT_3D('',#4618,#3671,#3672);
#3230=AXIS2_PLACEMENT_3D('',#4622,#3674,#3675);
#3231=AXIS2_PLACEMENT_3D('',#4624,#3677,#3678);
#3232=AXIS2_PLACEMENT_3D('',#4634,#3684,#3685);
#3233=AXIS2_PLACEMENT_3D('',#4638,#3688,#3689);
#3234=AXIS2_PLACEMENT_3D('',#4648,#3695,#3696);
#3235=AXIS2_PLACEMENT_3D('',#4652,#3699,#3700);
#3236=AXIS2_PLACEMENT_3D('',#4660,#3705,#3706);
#3237=AXIS2_PLACEMENT_3D('',#4662,#3708,#3709);
#3238=AXIS2_PLACEMENT_3D('',#4665,#3712,#3713);
#3239=AXIS2_PLACEMENT_3D('',#4666,#3714,#3715);
#3240=AXIS2_PLACEMENT_3D('',#4674,#3720,#3721);
#3241=AXIS2_PLACEMENT_3D('',#4676,#3723,#3724);
#3242=AXIS2_PLACEMENT_3D('',#4679,#3727,#3728);
#3243=AXIS2_PLACEMENT_3D('',#4680,#3729,#3730);
#3244=AXIS2_PLACEMENT_3D('',#4682,#3731,#3732);
#3245=AXIS2_PLACEMENT_3D('',#4685,#3734,#3735);
#3246=AXIS2_PLACEMENT_3D('',#4686,#3736,#3737);
#3247=AXIS2_PLACEMENT_3D('',#4688,#3738,#3739);
#3248=AXIS2_PLACEMENT_3D('',#4691,#3741,#3742);
#3249=AXIS2_PLACEMENT_3D('',#4692,#3743,#3744);
#3250=AXIS2_PLACEMENT_3D('',#4694,#3745,#3746);
#3251=AXIS2_PLACEMENT_3D('',#4697,#3748,#3749);
#3252=AXIS2_PLACEMENT_3D('',#4698,#3750,#3751);
#3253=AXIS2_PLACEMENT_3D('',#4700,#3752,#3753);
#3254=AXIS2_PLACEMENT_3D('',#4703,#3755,#3756);
#3255=AXIS2_PLACEMENT_3D('',#4704,#3757,#3758);
#3256=AXIS2_PLACEMENT_3D('',#4713,#3763,#3764);
#3257=AXIS2_PLACEMENT_3D('',#4719,#3768,#3769);
#3258=AXIS2_PLACEMENT_3D('',#4725,#3773,#3774);
#3259=AXIS2_PLACEMENT_3D('',#4728,#3777,#3778);
#3260=AXIS2_PLACEMENT_3D('',#4729,#3779,#3780);
#3261=AXIS2_PLACEMENT_3D('',#4730,#3781,#3782);
#3262=AXIS2_PLACEMENT_3D('',#4731,#3783,#3784);
#3263=AXIS2_PLACEMENT_3D('',#4733,#3785,#3786);
#3264=AXIS2_PLACEMENT_3D('',#4736,#3788,#3789);
#3265=AXIS2_PLACEMENT_3D('',#4737,#3790,#3791);
#3266=AXIS2_PLACEMENT_3D('',#4738,#3792,#3793);
#3267=AXIS2_PLACEMENT_3D('',#4740,#3794,#3795);
#3268=AXIS2_PLACEMENT_3D('',#4742,#3796,#3797);
#3269=AXIS2_PLACEMENT_3D('',#4743,#3798,#3799);
#3270=AXIS2_PLACEMENT_3D('',#4746,#3801,#3802);
#3271=AXIS2_PLACEMENT_3D('',#4747,#3803,#3804);
#3272=AXIS2_PLACEMENT_3D('',#4748,#3805,#3806);
#3273=AXIS2_PLACEMENT_3D('',#4750,#3807,#3808);
#3274=AXIS2_PLACEMENT_3D('',#4752,#3810,#3811);
#3275=AXIS2_PLACEMENT_3D('',#4753,#3812,#3813);
#3276=AXIS2_PLACEMENT_3D('',#4754,#3814,#3815);
#3277=AXIS2_PLACEMENT_3D('',#4756,#3816,#3817);
#3278=AXIS2_PLACEMENT_3D('',#4759,#3819,#3820);
#3279=AXIS2_PLACEMENT_3D('',#4760,#3821,#3822);
#3280=AXIS2_PLACEMENT_3D('',#4762,#3823,#3824);
#3281=AXIS2_PLACEMENT_3D('',#4765,#3826,#3827);
#3282=AXIS2_PLACEMENT_3D('',#4766,#3828,#3829);
#3283=AXIS2_PLACEMENT_3D('',#4767,#3830,#3831);
#3284=AXIS2_PLACEMENT_3D('',#4768,#3832,#3833);
#3285=AXIS2_PLACEMENT_3D('',#4769,#3834,#3835);
#3286=AXIS2_PLACEMENT_3D('',#4771,#3836,#3837);
#3287=AXIS2_PLACEMENT_3D('',#4774,#3839,#3840);
#3288=AXIS2_PLACEMENT_3D('',#4775,#3841,#3842);
#3289=AXIS2_PLACEMENT_3D('',#4777,#3843,#3844);
#3290=AXIS2_PLACEMENT_3D('',#4780,#3846,#3847);
#3291=AXIS2_PLACEMENT_3D('',#4781,#3848,#3849);
#3292=AXIS2_PLACEMENT_3D('',#4782,#3850,#3851);
#3293=AXIS2_PLACEMENT_3D('',#4783,#3852,#3853);
#3294=AXIS2_PLACEMENT_3D('',#4784,#3854,#3855);
#3295=AXIS2_PLACEMENT_3D('',#4793,#3860,#3861);
#3296=AXIS2_PLACEMENT_3D('',#4799,#3865,#3866);
#3297=AXIS2_PLACEMENT_3D('',#4805,#3870,#3871);
#3298=AXIS2_PLACEMENT_3D('',#4811,#3875,#3876);
#3299=AXIS2_PLACEMENT_3D('',#4817,#3880,#3881);
#3300=AXIS2_PLACEMENT_3D('',#4820,#3884,#3885);
#3301=AXIS2_PLACEMENT_3D('',#4821,#3886,#3887);
#3302=AXIS2_PLACEMENT_3D('',#4822,#3888,#3889);
#3303=AXIS2_PLACEMENT_3D('',#4824,#3890,#3891);
#3304=AXIS2_PLACEMENT_3D('',#4825,#3892,#3893);
#3305=AXIS2_PLACEMENT_3D('',#4827,#3894,#3895);
#3306=AXIS2_PLACEMENT_3D('',#4828,#3896,#3897);
#3307=AXIS2_PLACEMENT_3D('',#4830,#3898,#3899);
#3308=AXIS2_PLACEMENT_3D('',#4832,#3901,#3902);
#3309=AXIS2_PLACEMENT_3D('',#4834,#3903,#3904);
#3310=AXIS2_PLACEMENT_3D('',#4836,#3906,#3907);
#3311=AXIS2_PLACEMENT_3D('',#4838,#3908,#3909);
#3312=AXIS2_PLACEMENT_3D('',#4840,#3911,#3912);
#3313=AXIS2_PLACEMENT_3D('',#4842,#3913,#3914);
#3314=AXIS2_PLACEMENT_3D('',#4843,#3915,#3916);
#3315=AXIS2_PLACEMENT_3D('',#4845,#3917,#3918);
#3316=AXIS2_PLACEMENT_3D('',#4847,#3920,#3921);
#3317=AXIS2_PLACEMENT_3D('',#4849,#3923,#3924);
#3318=AXIS2_PLACEMENT_3D('',#4850,#3925,#3926);
#3319=AXIS2_PLACEMENT_3D('',#4852,#3927,#3928);
#3320=AXIS2_PLACEMENT_3D('',#4855,#3930,#3931);
#3321=AXIS2_PLACEMENT_3D('',#4856,#3932,#3933);
#3322=AXIS2_PLACEMENT_3D('',#4858,#3934,#3935);
#3323=AXIS2_PLACEMENT_3D('',#4861,#3937,#3938);
#3324=AXIS2_PLACEMENT_3D('',#4862,#3939,#3940);
#3325=AXIS2_PLACEMENT_3D('',#4863,#3941,#3942);
#3326=AXIS2_PLACEMENT_3D('',#4864,#3943,#3944);
#3327=AXIS2_PLACEMENT_3D('',#4865,#3945,#3946);
#3328=AXIS2_PLACEMENT_3D('',#4867,#3947,#3948);
#3329=AXIS2_PLACEMENT_3D('',#4870,#3950,#3951);
#3330=AXIS2_PLACEMENT_3D('',#4871,#3952,#3953);
#3331=AXIS2_PLACEMENT_3D('',#4873,#3954,#3955);
#3332=AXIS2_PLACEMENT_3D('',#4875,#3957,#3958);
#3333=AXIS2_PLACEMENT_3D('',#4876,#3959,#3960);
#3334=AXIS2_PLACEMENT_3D('',#4878,#3961,#3962);
#3335=AXIS2_PLACEMENT_3D('',#4904,#3964,#3965);
#3336=AXIS2_PLACEMENT_3D('',#4910,#3969,#3970);
#3337=AXIS2_PLACEMENT_3D('',#4914,#3973,#3974);
#3338=AXIS2_PLACEMENT_3D('',#4918,#3977,#3978);
#3339=AXIS2_PLACEMENT_3D('',#4922,#3981,#3982);
#3340=AXIS2_PLACEMENT_3D('',#4926,#3985,#3986);
#3341=AXIS2_PLACEMENT_3D('',#4928,#3988,#3989);
#3342=AXIS2_PLACEMENT_3D('',#4929,#3990,#3991);
#3343=AXIS2_PLACEMENT_3D('',#4930,#3992,#3993);
#3344=AXIS2_PLACEMENT_3D('',#4931,#3994,#3995);
#3345=AXIS2_PLACEMENT_3D('',#4943,#3997,#3998);
#3346=AXIS2_PLACEMENT_3D('',#4959,#3999,#4000);
#3347=AXIS2_PLACEMENT_3D('',#4961,#4001,#4002);
#3348=AXIS2_PLACEMENT_3D('',#4987,#4004,#4005);
#3349=AXIS2_PLACEMENT_3D('',#4990,#4008,#4009);
#3350=AXIS2_PLACEMENT_3D('',#4992,#4011,#4012);
#3351=AXIS2_PLACEMENT_3D('',#4994,#4014,#4015);
#3352=AXIS2_PLACEMENT_3D('',#4996,#4016,#4017);
#3353=AXIS2_PLACEMENT_3D('',#4999,#4019,#4020);
#3354=AXIS2_PLACEMENT_3D('',#5000,#4021,#4022);
#3355=AXIS2_PLACEMENT_3D('',#5002,#4024,#4025);
#3356=AXIS2_PLACEMENT_3D('',#5004,#4027,#4028);
#3357=AXIS2_PLACEMENT_3D('',#5005,#4029,#4030);
#3358=AXIS2_PLACEMENT_3D('',#5006,#4031,#4032);
#3359=AXIS2_PLACEMENT_3D('',#5007,#4033,#4034);
#3360=AXIS2_PLACEMENT_3D('',#5008,#4035,#4036);
#3361=AXIS2_PLACEMENT_3D('',#5009,#4037,#4038);
#3362=AXIS2_PLACEMENT_3D('',#5010,#4039,#4040);
#3363=AXIS2_PLACEMENT_3D('',#5011,#4041,#4042);
#3364=AXIS2_PLACEMENT_3D('',#5012,#4043,#4044);
#3365=AXIS2_PLACEMENT_3D('',#5013,#4045,#4046);
#3366=AXIS2_PLACEMENT_3D('',#5014,#4047,#4048);
#3367=AXIS2_PLACEMENT_3D('',#5015,#4049,#4050);
#3368=AXIS2_PLACEMENT_3D('',#5016,#4051,#4052);
#3369=AXIS2_PLACEMENT_3D('',#5017,#4053,#4054);
#3370=AXIS2_PLACEMENT_3D('',#5018,#4055,#4056);
#3371=AXIS2_PLACEMENT_3D('',#5019,#4057,#4058);
#3372=AXIS2_PLACEMENT_3D('',#5021,#4059,#4060);
#3373=AXIS2_PLACEMENT_3D('',#5024,#4062,#4063);
#3374=AXIS2_PLACEMENT_3D('',#5025,#4064,#4065);
#3375=AXIS2_PLACEMENT_3D('',#5027,#4066,#4067);
#3376=AXIS2_PLACEMENT_3D('',#5028,#4068,#4069);
#3377=AXIS2_PLACEMENT_3D('',#5030,#4070,#4071);
#3378=AXIS2_PLACEMENT_3D('',#5033,#4073,#4074);
#3379=AXIS2_PLACEMENT_3D('',#5034,#4075,#4076);
#3380=AXIS2_PLACEMENT_3D('',#5036,#4077,#4078);
#3381=AXIS2_PLACEMENT_3D('',#5037,#4079,#4080);
#3382=AXIS2_PLACEMENT_3D('',#5039,#4082,#4083);
#3383=AXIS2_PLACEMENT_3D('',#5041,#4084,#4085);
#3384=AXIS2_PLACEMENT_3D('',#5044,#4087,#4088);
#3385=AXIS2_PLACEMENT_3D('',#5045,#4089,#4090);
#3386=AXIS2_PLACEMENT_3D('',#5046,#4091,#4092);
#3387=AXIS2_PLACEMENT_3D('',#5047,#4093,#4094);
#3388=AXIS2_PLACEMENT_3D('',#5048,#4095,#4096);
#3389=AXIS2_PLACEMENT_3D('',#5049,#4097,#4098);
#3390=AXIS2_PLACEMENT_3D('',#5052,#4099,#4100);
#3391=AXIS2_PLACEMENT_3D('',#5053,#4101,#4102);
#3392=AXIS2_PLACEMENT_3D('',#5055,#4103,#4104);
#3393=AXIS2_PLACEMENT_3D('',#5057,#4105,#4106);
#3394=AXIS2_PLACEMENT_3D('',#5058,#4107,#4108);
#3395=AXIS2_PLACEMENT_3D('',#5059,#4109,#4110);
#3396=AXIS2_PLACEMENT_3D('',#5062,#4112,#4113);
#3397=AXIS2_PLACEMENT_3D('',#5063,#4114,#4115);
#3398=AXIS2_PLACEMENT_3D('',#5065,#4116,#4117);
#3399=AXIS2_PLACEMENT_3D('',#5068,#4119,#4120);
#3400=AXIS2_PLACEMENT_3D('',#5069,#4121,#4122);
#3401=AXIS2_PLACEMENT_3D('',#5072,#4124,#4125);
#3402=AXIS2_PLACEMENT_3D('',#5073,#4126,#4127);
#3403=AXIS2_PLACEMENT_3D('',#5074,#4128,#4129);
#3404=AXIS2_PLACEMENT_3D('',#5076,#4130,#4131);
#3405=AXIS2_PLACEMENT_3D('',#5078,#4133,#4134);
#3406=AXIS2_PLACEMENT_3D('',#5080,#4135,#4136);
#3407=AXIS2_PLACEMENT_3D('',#5081,#4137,#4138);
#3408=AXIS2_PLACEMENT_3D('',#5083,#4140,#4141);
#3409=AXIS2_PLACEMENT_3D('',#5084,#4142,#4143);
#3410=AXIS2_PLACEMENT_3D('',#5087,#4144,#4145);
#3411=AXIS2_PLACEMENT_3D('',#5088,#4146,#4147);
#3412=AXIS2_PLACEMENT_3D('',#5090,#4148,#4149);
#3413=AXIS2_PLACEMENT_3D('',#5092,#4150,#4151);
#3414=AXIS2_PLACEMENT_3D('',#5093,#4152,#4153);
#3415=AXIS2_PLACEMENT_3D('',#5094,#4154,#4155);
#3416=AXIS2_PLACEMENT_3D('',#5096,#4156,#4157);
#3417=AXIS2_PLACEMENT_3D('',#5098,#4159,#4160);
#3418=AXIS2_PLACEMENT_3D('',#5100,#4161,#4162);
#3419=AXIS2_PLACEMENT_3D('',#5102,#4163,#4164);
#3420=AXIS2_PLACEMENT_3D('',#5103,#4165,#4166);
#3421=AXIS2_PLACEMENT_3D('',#5105,#4167,#4168);
#3422=AXIS2_PLACEMENT_3D('',#5107,#4170,#4171);
#3423=AXIS2_PLACEMENT_3D('',#5109,#4172,#4173);
#3424=AXIS2_PLACEMENT_3D('',#5111,#4175,#4176);
#3425=AXIS2_PLACEMENT_3D('',#5113,#4177,#4178);
#3426=AXIS2_PLACEMENT_3D('',#5115,#4180,#4181);
#3427=AXIS2_PLACEMENT_3D('',#5116,#4182,#4183);
#3428=AXIS2_PLACEMENT_3D('',#5118,#4185,#4186);
#3429=AXIS2_PLACEMENT_3D('',#5119,#4187,#4188);
#3430=AXIS2_PLACEMENT_3D('',#5122,#4189,#4190);
#3431=AXIS2_PLACEMENT_3D('',#5123,#4191,#4192);
#3432=AXIS2_PLACEMENT_3D('',#5126,#4193,#4194);
#3433=AXIS2_PLACEMENT_3D('',#5127,#4195,#4196);
#3434=AXIS2_PLACEMENT_3D('',#5130,#4197,#4198);
#3435=AXIS2_PLACEMENT_3D('',#5131,#4199,#4200);
#3436=AXIS2_PLACEMENT_3D('',#5134,#4201,#4202);
#3437=AXIS2_PLACEMENT_3D('',#5135,#4203,#4204);
#3438=AXIS2_PLACEMENT_3D('',#5138,#4205,#4206);
#3439=AXIS2_PLACEMENT_3D('',#5139,#4207,#4208);
#3440=AXIS2_PLACEMENT_3D('',#5142,#4209,#4210);
#3441=AXIS2_PLACEMENT_3D('',#5143,#4211,#4212);
#3442=AXIS2_PLACEMENT_3D('',#5146,#4213,#4214);
#3443=AXIS2_PLACEMENT_3D('',#5147,#4215,#4216);
#3444=AXIS2_PLACEMENT_3D('',#5148,#4217,#4218);
#3445=AXIS2_PLACEMENT_3D('',#5174,#4219,#4220);
#3446=AXIS2_PLACEMENT_3D('',#5198,#4221,#4222);
#3447=AXIS2_PLACEMENT_3D('',#5199,#4223,#4224);
#3448=AXIS2_PLACEMENT_3D('',#5201,#4225,#4226);
#3449=AXIS2_PLACEMENT_3D('',#5226,#4227,#4228);
#3450=AXIS2_PLACEMENT_3D('',#5251,#4229,#4230);
#3451=AXIS2_PLACEMENT_3D('',#5254,#4232,#4233);
#3452=AXIS2_PLACEMENT_3D('',#5256,#4234,#4235);
#3453=AXIS2_PLACEMENT_3D('',#5281,#4236,#4237);
#3454=AXIS2_PLACEMENT_3D('',#5306,#4238,#4239);
#3455=AXIS2_PLACEMENT_3D('',#5331,#4240,#4241);
#3456=AXIS2_PLACEMENT_3D('',#5355,#4242,#4243);
#3457=AXIS2_PLACEMENT_3D('',#5356,#4244,#4245);
#3458=AXIS2_PLACEMENT_3D('',#5358,#4246,#4247);
#3459=AXIS2_PLACEMENT_3D('',#5359,#4248,#4249);
#3460=AXIS2_PLACEMENT_3D('',#5360,#4250,#4251);
#3461=AXIS2_PLACEMENT_3D('',#5384,#4252,#4253);
#3462=AXIS2_PLACEMENT_3D('',#5385,#4254,#4255);
#3463=AXIS2_PLACEMENT_3D('',#5387,#4256,#4257);
#3464=AXIS2_PLACEMENT_3D('',#5388,#4258,#4259);
#3465=AXIS2_PLACEMENT_3D('',#5389,#4260,#4261);
#3466=AXIS2_PLACEMENT_3D('',#5413,#4262,#4263);
#3467=AXIS2_PLACEMENT_3D('',#5414,#4264,#4265);
#3468=AXIS2_PLACEMENT_3D('',#5416,#4266,#4267);
#3469=AXIS2_PLACEMENT_3D('',#5418,#4268,#4269);
#3470=AXIS2_PLACEMENT_3D('',#5419,#4270,#4271);
#3471=AXIS2_PLACEMENT_3D('',#5420,#4272,#4273);
#3472=AXIS2_PLACEMENT_3D('',#5444,#4274,#4275);
#3473=AXIS2_PLACEMENT_3D('',#5445,#4276,#4277);
#3474=AXIS2_PLACEMENT_3D('',#5447,#4278,#4279);
#3475=AXIS2_PLACEMENT_3D('',#5448,#4280,#4281);
#3476=AXIS2_PLACEMENT_3D('',#5449,#4282,#4283);
#3477=AXIS2_PLACEMENT_3D('',#5473,#4284,#4285);
#3478=AXIS2_PLACEMENT_3D('',#5474,#4286,#4287);
#3479=AXIS2_PLACEMENT_3D('',#5476,#4288,#4289);
#3480=AXIS2_PLACEMENT_3D('',#5477,#4290,#4291);
#3481=AXIS2_PLACEMENT_3D('',#5478,#4292,#4293);
#3482=AXIS2_PLACEMENT_3D('',#5502,#4294,#4295);
#3483=AXIS2_PLACEMENT_3D('',#5503,#4296,#4297);
#3484=AXIS2_PLACEMENT_3D('',#5505,#4298,#4299);
#3485=AXIS2_PLACEMENT_3D('',#5508,#4301,#4302);
#3486=AXIS2_PLACEMENT_3D('',#5532,#4303,#4304);
#3487=AXIS2_PLACEMENT_3D('',#5533,#4305,#4306);
#3488=AXIS2_PLACEMENT_3D('',#5534,#4307,#4308);
#3489=AXIS2_PLACEMENT_3D('',#5535,#4309,#4310);
#3490=AXIS2_PLACEMENT_3D('',#5536,#4311,#4312);
#3491=AXIS2_PLACEMENT_3D('',#5537,#4313,#4314);
#3492=AXIS2_PLACEMENT_3D('',#5538,#4315,#4316);
#3493=AXIS2_PLACEMENT_3D('',#5539,#4317,#4318);
#3494=AXIS2_PLACEMENT_3D('',#5540,#4319,#4320);
#3495=AXIS2_PLACEMENT_3D('',#5542,#4321,#4322);
#3496=AXIS2_PLACEMENT_3D('',#5544,#4323,#4324);
#3497=AXIS2_PLACEMENT_3D('',#5545,#4325,#4326);
#3498=AXIS2_PLACEMENT_3D('',#5547,#4327,#4328);
#3499=AXIS2_PLACEMENT_3D('',#5549,#4330,#4331);
#3500=AXIS2_PLACEMENT_3D('',#5551,#4332,#4333);
#3501=AXIS2_PLACEMENT_3D('',#5552,#4334,#4335);
#3502=AXIS2_PLACEMENT_3D('',#5554,#4337,#4338);
#3503=AXIS2_PLACEMENT_3D('',#5556,#4339,#4340);
#3504=AXIS2_PLACEMENT_3D('',#5558,#4341,#4342);
#3505=AXIS2_PLACEMENT_3D('',#5559,#4343,#4344);
#3506=AXIS2_PLACEMENT_3D('',#5561,#4345,#4346);
#3507=AXIS2_PLACEMENT_3D('',#5563,#4348,#4349);
#3508=AXIS2_PLACEMENT_3D('',#5565,#4350,#4351);
#3509=AXIS2_PLACEMENT_3D('',#5566,#4352,#4353);
#3510=AXIS2_PLACEMENT_3D('',#5568,#4355,#4356);
#3511=AXIS2_PLACEMENT_3D('',#5569,#4357,#4358);
#3512=AXIS2_PLACEMENT_3D('',#5570,#4359,#4360);
#3513=AXIS2_PLACEMENT_3D('',#5571,#4361,#4362);
#3514=AXIS2_PLACEMENT_3D('',#5572,#4363,#4364);
#3515=AXIS2_PLACEMENT_3D('',#5573,#4365,#4366);
#3516=AXIS2_PLACEMENT_3D('',#5574,#4367,#4368);
#3517=AXIS2_PLACEMENT_3D('',#5576,#4369,#4370);
#3518=AXIS2_PLACEMENT_3D('',#5579,#4372,#4373);
#3519=AXIS2_PLACEMENT_3D('',#5580,#4374,#4375);
#3520=AXIS2_PLACEMENT_3D('',#5582,#4376,#4377);
#3521=AXIS2_PLACEMENT_3D('',#5585,#4379,#4380);
#3522=AXIS2_PLACEMENT_3D('',#5586,#4381,#4382);
#3523=AXIS2_PLACEMENT_3D('',#5587,#4383,#4384);
#3524=AXIS2_PLACEMENT_3D('',#5588,#4385,#4386);
#3525=AXIS2_PLACEMENT_3D('',#5589,#4387,#4388);
#3526=AXIS2_PLACEMENT_3D('',#5590,#4389,#4390);
#3527=AXIS2_PLACEMENT_3D('',#5591,#4391,#4392);
#3528=AXIS2_PLACEMENT_3D('',#5592,#4393,#4394);
#3529=AXIS2_PLACEMENT_3D('',#5593,#4395,#4396);
#3530=AXIS2_PLACEMENT_3D('',#5594,#4397,#4398);
#3531=AXIS2_PLACEMENT_3D('',#5595,#4399,#4400);
#3532=AXIS2_PLACEMENT_3D('',#5597,#4401,#4402);
#3533=AXIS2_PLACEMENT_3D('',#5600,#4404,#4405);
#3534=AXIS2_PLACEMENT_3D('',#5601,#4406,#4407);
#3535=AXIS2_PLACEMENT_3D('',#5610,#4412,#4413);
#3536=AXIS2_PLACEMENT_3D('',#5616,#4417,#4418);
#3537=AXIS2_PLACEMENT_3D('',#5622,#4422,#4423);
#3538=AXIS2_PLACEMENT_3D('',#5624,#4424,#4425);
#3539=AXIS2_PLACEMENT_3D('',#5633,#4430,#4431);
#3540=AXIS2_PLACEMENT_3D('',#5634,#4432,#4433);
#3541=AXIS2_PLACEMENT_3D('',#5636,#4434,#4435);
#3542=AXIS2_PLACEMENT_3D('',#5638,#4437,#4438);
#3543=AXIS2_PLACEMENT_3D('',#5644,#4442,#4443);
#3544=AXIS2_PLACEMENT_3D('',#5648,#4446,#4447);
#3545=AXIS2_PLACEMENT_3D('',#5652,#4450,#4451);
#3546=AXIS2_PLACEMENT_3D('',#5654,#4453,#4454);
#3547=AXIS2_PLACEMENT_3D('',#5655,#4455,#4456);
#3548=AXIS2_PLACEMENT_3D('',#5656,#4457,#4458);
#3549=AXIS2_PLACEMENT_3D('',#5657,#4459,#4460);
#3550=AXIS2_PLACEMENT_3D('',#5658,#4461,#4462);
#3551=AXIS2_PLACEMENT_3D('',#5667,#4467,#4468);
#3552=AXIS2_PLACEMENT_3D('',#5673,#4472,#4473);
#3553=AXIS2_PLACEMENT_3D('',#5679,#4477,#4478);
#3554=AXIS2_PLACEMENT_3D('',#5682,#4481,#4482);
#3555=AXIS2_PLACEMENT_3D('',#5683,#4483,#4484);
#3556=AXIS2_PLACEMENT_3D('',#5684,#4485,#4486);
#3557=AXIS2_PLACEMENT_3D('',#5685,#4487,#4488);
#3558=AXIS2_PLACEMENT_3D('',#5686,#4489,#4490);
#3559=AXIS2_PLACEMENT_3D('',#5687,#4491,#4492);
#3560=AXIS2_PLACEMENT_3D('',#5688,#4493,#4494);
#3561=DIRECTION('axis',(0.,0.,1.));
#3562=DIRECTION('refdir',(1.,0.,0.));
#3563=DIRECTION('axis',(0.,0.,1.));
#3564=DIRECTION('refdir',(1.,0.,0.));
#3565=DIRECTION('axis',(0.,0.,1.));
#3566=DIRECTION('refdir',(1.,0.,0.));
#3567=DIRECTION('center_axis',(-1.,0.,0.));
#3568=DIRECTION('ref_axis',(0.,-1.,0.));
#3569=DIRECTION('',(0.,1.,0.));
#3570=DIRECTION('',(0.,0.,1.));
#3571=DIRECTION('',(0.,-1.,0.));
#3572=DIRECTION('',(0.,0.,1.));
#3573=DIRECTION('center_axis',(0.,-1.,0.));
#3574=DIRECTION('ref_axis',(1.,0.,0.));
#3575=DIRECTION('',(-1.,0.,0.));
#3576=DIRECTION('',(0.,0.,1.));
#3577=DIRECTION('',(1.,0.,0.));
#3578=DIRECTION('',(0.,0.,1.));
#3579=DIRECTION('',(1.,0.,0.));
#3580=DIRECTION('',(0.,0.,-1.));
#3581=DIRECTION('',(1.,0.,0.));
#3582=DIRECTION('center_axis',(0.,0.,1.));
#3583=DIRECTION('ref_axis',(1.,0.,0.));
#3584=DIRECTION('',(0.,-1.,0.));
#3585=DIRECTION('',(1.,0.,0.));
#3586=DIRECTION('',(0.,1.,0.));
#3587=DIRECTION('center_axis',(0.,0.,1.));
#3588=DIRECTION('ref_axis',(1.,0.,0.));
#3589=DIRECTION('',(0.,-1.,0.));
#3590=DIRECTION('',(-1.,0.,0.));
#3591=DIRECTION('',(0.,1.,0.));
#3592=DIRECTION('',(-1.,0.,0.));
#3593=DIRECTION('center_axis',(0.,1.,0.));
#3594=DIRECTION('ref_axis',(-1.,0.,0.));
#3595=DIRECTION('',(1.,0.,0.));
#3596=DIRECTION('',(-1.,0.,0.));
#3597=DIRECTION('',(0.,0.,1.));
#3598=DIRECTION('',(0.,0.,-1.));
#3599=DIRECTION('',(-1.,0.,0.));
#3600=DIRECTION('',(0.,0.,1.));
#3601=DIRECTION('center_axis',(1.,0.,0.));
#3602=DIRECTION('ref_axis',(0.,1.,0.));
#3603=DIRECTION('',(0.,-1.,0.));
#3604=DIRECTION('',(0.,1.,0.));
#3605=DIRECTION('center_axis',(0.,1.,0.));
#3606=DIRECTION('ref_axis',(1.,0.,0.));
#3607=DIRECTION('',(0.,0.,-1.));
#3608=DIRECTION('',(1.,0.,0.));
#3609=DIRECTION('',(0.,0.,1.));
#3610=DIRECTION('center_axis',(0.,1.,0.));
#3611=DIRECTION('ref_axis',(1.,0.,0.));
#3612=DIRECTION('center_axis',(-1.,0.,0.));
#3613=DIRECTION('ref_axis',(0.,0.,1.));
#3614=DIRECTION('',(0.,-1.,0.));
#3615=DIRECTION('',(0.,0.,1.));
#3616=DIRECTION('',(0.,1.,0.));
#3617=DIRECTION('center_axis',(-1.,0.,0.));
#3618=DIRECTION('ref_axis',(0.,0.,1.));
#3619=DIRECTION('',(0.,0.,1.));
#3620=DIRECTION('',(0.,1.,0.));
#3621=DIRECTION('',(0.,0.,-1.));
#3622=DIRECTION('',(0.,-1.,0.));
#3623=DIRECTION('center_axis',(0.,1.,0.));
#3624=DIRECTION('ref_axis',(1.,0.,0.));
#3625=DIRECTION('center_axis',(0.,1.,0.));
#3626=DIRECTION('ref_axis',(1.,0.,0.));
#3627=DIRECTION('',(0.,1.,0.));
#3628=DIRECTION('center_axis',(0.,-1.,0.));
#3629=DIRECTION('ref_axis',(1.,0.,0.));
#3630=DIRECTION('center_axis',(0.,1.,0.));
#3631=DIRECTION('ref_axis',(1.,0.,0.));
#3632=DIRECTION('',(0.,1.,0.));
#3633=DIRECTION('center_axis',(0.,-1.,0.));
#3634=DIRECTION('ref_axis',(1.,0.,0.));
#3635=DIRECTION('center_axis',(0.,1.,0.));
#3636=DIRECTION('ref_axis',(0.,0.,1.));
#3637=DIRECTION('',(-1.,0.,0.));
#3638=DIRECTION('',(0.,0.,-1.));
#3639=DIRECTION('',(-1.,0.,0.));
#3640=DIRECTION('center_axis',(1.,0.,0.));
#3641=DIRECTION('ref_axis',(0.,0.,-1.));
#3642=DIRECTION('',(0.,1.,0.));
#3643=DIRECTION('',(0.,1.,0.));
#3644=DIRECTION('center_axis',(0.,0.,-1.));
#3645=DIRECTION('ref_axis',(-1.,0.,0.));
#3646=DIRECTION('center_axis',(0.,1.,0.));
#3647=DIRECTION('ref_axis',(0.,0.,1.));
#3648=DIRECTION('',(0.,0.,-1.));
#3649=DIRECTION('',(-1.,0.,0.));
#3650=DIRECTION('center_axis',(1.,0.,0.));
#3651=DIRECTION('ref_axis',(0.,0.,-1.));
#3652=DIRECTION('',(0.,1.,0.));
#3653=DIRECTION('',(0.,0.,1.));
#3654=DIRECTION('',(0.,1.,0.));
#3655=DIRECTION('center_axis',(0.,0.,-1.));
#3656=DIRECTION('ref_axis',(-1.,0.,0.));
#3657=DIRECTION('',(1.,0.,0.));
#3658=DIRECTION('center_axis',(0.,1.,0.));
#3659=DIRECTION('ref_axis',(1.,0.,0.));
#3660=DIRECTION('',(1.,0.,0.));
#3661=DIRECTION('center_axis',(0.,1.,0.));
#3662=DIRECTION('ref_axis',(1.,0.,0.));
#3663=DIRECTION('center_axis',(0.,-1.,0.));
#3664=DIRECTION('ref_axis',(1.,0.,0.));
#3665=DIRECTION('',(0.,1.,0.));
#3666=DIRECTION('center_axis',(0.,1.,0.));
#3667=DIRECTION('ref_axis',(1.,0.,0.));
#3668=DIRECTION('',(0.,-1.,0.));
#3669=DIRECTION('center_axis',(0.,1.,0.));
#3670=DIRECTION('ref_axis',(1.,0.,0.));
#3671=DIRECTION('center_axis',(0.,-1.,0.));
#3672=DIRECTION('ref_axis',(1.,0.,0.));
#3673=DIRECTION('',(0.,1.,0.));
#3674=DIRECTION('center_axis',(0.,1.,0.));
#3675=DIRECTION('ref_axis',(1.,0.,0.));
#3676=DIRECTION('',(0.,-1.,0.));
#3677=DIRECTION('center_axis',(0.,1.,0.));
#3678=DIRECTION('ref_axis',(1.,0.,0.));
#3679=DIRECTION('',(1.,0.,0.));
#3680=DIRECTION('',(0.,0.,1.));
#3681=DIRECTION('',(1.,0.,0.));
#3682=DIRECTION('',(0.,0.,-1.));
#3683=DIRECTION('',(1.,0.,0.));
#3684=DIRECTION('center_axis',(0.,0.,-1.));
#3685=DIRECTION('ref_axis',(-1.,0.,0.));
#3686=DIRECTION('',(-1.,0.,0.));
#3687=DIRECTION('',(0.,1.,0.));
#3688=DIRECTION('center_axis',(0.,1.,0.));
#3689=DIRECTION('ref_axis',(1.,0.,0.));
#3690=DIRECTION('',(1.,0.,0.));
#3691=DIRECTION('',(0.,0.,1.));
#3692=DIRECTION('',(1.,0.,0.));
#3693=DIRECTION('',(0.,0.,-1.));
#3694=DIRECTION('',(1.,0.,0.));
#3695=DIRECTION('center_axis',(0.,0.,-1.));
#3696=DIRECTION('ref_axis',(-1.,0.,0.));
#3697=DIRECTION('',(-1.,0.,0.));
#3698=DIRECTION('',(0.,1.,0.));
#3699=DIRECTION('center_axis',(0.,1.,0.));
#3700=DIRECTION('ref_axis',(0.,0.,1.));
#3701=DIRECTION('',(-1.,0.,0.));
#3702=DIRECTION('',(0.,0.,1.));
#3703=DIRECTION('',(-1.,0.,0.));
#3704=DIRECTION('',(0.,0.,-1.));
#3705=DIRECTION('center_axis',(1.,0.,0.));
#3706=DIRECTION('ref_axis',(0.,0.,-1.));
#3707=DIRECTION('',(0.,1.,0.));
#3708=DIRECTION('center_axis',(-1.,0.,0.));
#3709=DIRECTION('ref_axis',(0.,0.,1.));
#3710=DIRECTION('',(0.,-1.,0.));
#3711=DIRECTION('',(0.,1.,0.));
#3712=DIRECTION('center_axis',(0.,0.,-1.));
#3713=DIRECTION('ref_axis',(-1.,0.,0.));
#3714=DIRECTION('center_axis',(0.,1.,0.));
#3715=DIRECTION('ref_axis',(0.,0.,1.));
#3716=DIRECTION('',(-1.,0.,0.));
#3717=DIRECTION('',(0.,0.,1.));
#3718=DIRECTION('',(-1.,0.,0.));
#3719=DIRECTION('',(0.,0.,-1.));
#3720=DIRECTION('center_axis',(1.,0.,0.));
#3721=DIRECTION('ref_axis',(0.,0.,-1.));
#3722=DIRECTION('',(0.,1.,0.));
#3723=DIRECTION('center_axis',(-1.,0.,0.));
#3724=DIRECTION('ref_axis',(0.,0.,1.));
#3725=DIRECTION('',(0.,-1.,0.));
#3726=DIRECTION('',(0.,1.,0.));
#3727=DIRECTION('center_axis',(0.,0.,-1.));
#3728=DIRECTION('ref_axis',(-1.,0.,0.));
#3729=DIRECTION('center_axis',(0.,0.,1.));
#3730=DIRECTION('ref_axis',(1.,0.,0.));
#3731=DIRECTION('center_axis',(0.,0.,1.));
#3732=DIRECTION('ref_axis',(1.,0.,0.));
#3733=DIRECTION('',(0.,0.,1.));
#3734=DIRECTION('center_axis',(0.,0.,-1.));
#3735=DIRECTION('ref_axis',(1.,0.,0.));
#3736=DIRECTION('center_axis',(0.,0.,1.));
#3737=DIRECTION('ref_axis',(1.,0.,0.));
#3738=DIRECTION('center_axis',(0.,0.,1.));
#3739=DIRECTION('ref_axis',(1.,0.,0.));
#3740=DIRECTION('',(0.,0.,1.));
#3741=DIRECTION('center_axis',(0.,0.,-1.));
#3742=DIRECTION('ref_axis',(1.,0.,0.));
#3743=DIRECTION('center_axis',(0.,0.,1.));
#3744=DIRECTION('ref_axis',(1.,0.,0.));
#3745=DIRECTION('center_axis',(0.,0.,1.));
#3746=DIRECTION('ref_axis',(1.,0.,0.));
#3747=DIRECTION('',(0.,0.,1.));
#3748=DIRECTION('center_axis',(0.,0.,-1.));
#3749=DIRECTION('ref_axis',(1.,0.,0.));
#3750=DIRECTION('center_axis',(0.,0.,1.));
#3751=DIRECTION('ref_axis',(1.,0.,0.));
#3752=DIRECTION('center_axis',(0.,0.,1.));
#3753=DIRECTION('ref_axis',(1.,0.,0.));
#3754=DIRECTION('',(0.,0.,1.));
#3755=DIRECTION('center_axis',(0.,0.,-1.));
#3756=DIRECTION('ref_axis',(1.,0.,0.));
#3757=DIRECTION('center_axis',(0.,1.,0.));
#3758=DIRECTION('ref_axis',(-1.,0.,0.));
#3759=DIRECTION('',(-1.,0.,0.));
#3760=DIRECTION('',(0.,0.,1.));
#3761=DIRECTION('',(-1.,0.,0.));
#3762=DIRECTION('',(0.,0.,1.));
#3763=DIRECTION('center_axis',(1.,0.,0.));
#3764=DIRECTION('ref_axis',(0.,1.,0.));
#3765=DIRECTION('',(0.,1.,0.));
#3766=DIRECTION('',(0.,1.,0.));
#3767=DIRECTION('',(0.,0.,1.));
#3768=DIRECTION('center_axis',(0.,-1.,0.));
#3769=DIRECTION('ref_axis',(1.,0.,0.));
#3770=DIRECTION('',(1.,0.,0.));
#3771=DIRECTION('',(1.,0.,0.));
#3772=DIRECTION('',(0.,0.,1.));
#3773=DIRECTION('center_axis',(-1.,0.,0.));
#3774=DIRECTION('ref_axis',(0.,-1.,0.));
#3775=DIRECTION('',(0.,-1.,0.));
#3776=DIRECTION('',(0.,-1.,0.));
#3777=DIRECTION('center_axis',(0.,0.,1.));
#3778=DIRECTION('ref_axis',(1.,0.,0.));
#3779=DIRECTION('center_axis',(0.,0.,1.));
#3780=DIRECTION('ref_axis',(1.,0.,0.));
#3781=DIRECTION('axis',(0.,0.,1.));
#3782=DIRECTION('refdir',(1.,0.,0.));
#3783=DIRECTION('center_axis',(0.,1.,0.));
#3784=DIRECTION('ref_axis',(1.,0.,0.));
#3785=DIRECTION('center_axis',(0.,1.,0.));
#3786=DIRECTION('ref_axis',(1.,0.,0.));
#3787=DIRECTION('',(0.,1.,0.));
#3788=DIRECTION('center_axis',(0.,-1.,0.));
#3789=DIRECTION('ref_axis',(1.,0.,0.));
#3790=DIRECTION('center_axis',(0.,1.,0.));
#3791=DIRECTION('ref_axis',(1.,0.,0.));
#3792=DIRECTION('center_axis',(0.,1.,0.));
#3793=DIRECTION('ref_axis',(1.,0.,0.));
#3794=DIRECTION('center_axis',(0.,1.,0.));
#3795=DIRECTION('ref_axis',(1.,0.,0.));
#3796=DIRECTION('center_axis',(0.,1.,0.));
#3797=DIRECTION('ref_axis',(1.,0.,0.));
#3798=DIRECTION('center_axis',(0.,1.,0.));
#3799=DIRECTION('ref_axis',(1.,0.,0.));
#3800=DIRECTION('',(0.,-1.,0.));
#3801=DIRECTION('center_axis',(0.,1.,0.));
#3802=DIRECTION('ref_axis',(1.,0.,0.));
#3803=DIRECTION('center_axis',(0.,1.,0.));
#3804=DIRECTION('ref_axis',(1.,0.,0.));
#3805=DIRECTION('center_axis',(0.,1.,0.));
#3806=DIRECTION('ref_axis',(1.,0.,0.));
#3807=DIRECTION('center_axis',(0.,1.,0.));
#3808=DIRECTION('ref_axis',(1.,0.,0.));
#3809=DIRECTION('',(0.,-1.,0.));
#3810=DIRECTION('center_axis',(0.,1.,0.));
#3811=DIRECTION('ref_axis',(1.,0.,0.));
#3812=DIRECTION('axis',(0.,0.,1.));
#3813=DIRECTION('refdir',(1.,0.,0.));
#3814=DIRECTION('center_axis',(0.,1.,0.));
#3815=DIRECTION('ref_axis',(1.,0.,0.));
#3816=DIRECTION('center_axis',(0.,-1.,0.));
#3817=DIRECTION('ref_axis',(1.,0.,0.));
#3818=DIRECTION('',(0.,-1.,0.));
#3819=DIRECTION('center_axis',(0.,-1.,0.));
#3820=DIRECTION('ref_axis',(1.,0.,0.));
#3821=DIRECTION('center_axis',(0.,1.,0.));
#3822=DIRECTION('ref_axis',(1.,0.,0.));
#3823=DIRECTION('center_axis',(0.,1.,0.));
#3824=DIRECTION('ref_axis',(1.,0.,0.));
#3825=DIRECTION('',(0.,-1.,0.));
#3826=DIRECTION('center_axis',(0.,1.,0.));
#3827=DIRECTION('ref_axis',(1.,0.,0.));
#3828=DIRECTION('center_axis',(0.,1.,0.));
#3829=DIRECTION('ref_axis',(1.,0.,0.));
#3830=DIRECTION('center_axis',(0.,1.,0.));
#3831=DIRECTION('ref_axis',(1.,0.,0.));
#3832=DIRECTION('axis',(0.,0.,1.));
#3833=DIRECTION('refdir',(1.,0.,0.));
#3834=DIRECTION('center_axis',(0.,1.,0.));
#3835=DIRECTION('ref_axis',(1.,0.,0.));
#3836=DIRECTION('center_axis',(0.,-1.,0.));
#3837=DIRECTION('ref_axis',(1.,0.,0.));
#3838=DIRECTION('',(0.,-1.,0.));
#3839=DIRECTION('center_axis',(0.,-1.,0.));
#3840=DIRECTION('ref_axis',(1.,0.,0.));
#3841=DIRECTION('center_axis',(0.,1.,0.));
#3842=DIRECTION('ref_axis',(1.,0.,0.));
#3843=DIRECTION('center_axis',(0.,1.,0.));
#3844=DIRECTION('ref_axis',(1.,0.,0.));
#3845=DIRECTION('',(0.,-1.,0.));
#3846=DIRECTION('center_axis',(0.,1.,0.));
#3847=DIRECTION('ref_axis',(1.,0.,0.));
#3848=DIRECTION('center_axis',(0.,1.,0.));
#3849=DIRECTION('ref_axis',(1.,0.,0.));
#3850=DIRECTION('center_axis',(0.,1.,0.));
#3851=DIRECTION('ref_axis',(1.,0.,0.));
#3852=DIRECTION('axis',(0.,0.,1.));
#3853=DIRECTION('refdir',(1.,0.,0.));
#3854=DIRECTION('center_axis',(0.866025403784439,0.,-0.5));
#3855=DIRECTION('ref_axis',(0.5,0.,0.866025403784439));
#3856=DIRECTION('',(-0.5,0.,-0.866025403784439));
#3857=DIRECTION('',(0.,-1.,0.));
#3858=DIRECTION('',(0.5,0.,0.866025403784439));
#3859=DIRECTION('',(0.,-1.,0.));
#3860=DIRECTION('center_axis',(1.60246890531964E-16,0.,-1.));
#3861=DIRECTION('ref_axis',(1.,0.,1.60246890531964E-16));
#3862=DIRECTION('',(-1.,0.,-1.60246890531964E-16));
#3863=DIRECTION('',(0.,-1.,0.));
#3864=DIRECTION('',(1.,0.,1.60246890531964E-16));
#3865=DIRECTION('center_axis',(-0.866025403784439,0.,-0.5));
#3866=DIRECTION('ref_axis',(0.5,0.,-0.866025403784439));
#3867=DIRECTION('',(-0.5,0.,0.866025403784439));
#3868=DIRECTION('',(0.,-1.,0.));
#3869=DIRECTION('',(0.5,0.,-0.866025403784439));
#3870=DIRECTION('center_axis',(-0.866025403784439,0.,0.5));
#3871=DIRECTION('ref_axis',(-0.5,0.,-0.866025403784439));
#3872=DIRECTION('',(0.5,0.,0.866025403784439));
#3873=DIRECTION('',(0.,-1.,0.));
#3874=DIRECTION('',(-0.5,0.,-0.866025403784439));
#3875=DIRECTION('center_axis',(-1.60246890531964E-16,0.,1.));
#3876=DIRECTION('ref_axis',(-1.,0.,-1.60246890531964E-16));
#3877=DIRECTION('',(1.,0.,1.60246890531964E-16));
#3878=DIRECTION('',(0.,-1.,0.));
#3879=DIRECTION('',(-1.,0.,-1.60246890531964E-16));
#3880=DIRECTION('center_axis',(0.866025403784439,0.,0.5));
#3881=DIRECTION('ref_axis',(-0.5,0.,0.866025403784439));
#3882=DIRECTION('',(0.5,0.,-0.866025403784439));
#3883=DIRECTION('',(-0.5,0.,0.866025403784439));
#3884=DIRECTION('center_axis',(0.,1.,0.));
#3885=DIRECTION('ref_axis',(1.,0.,0.));
#3886=DIRECTION('center_axis',(0.,-1.,0.));
#3887=DIRECTION('ref_axis',(0.,0.,-1.));
#3888=DIRECTION('center_axis',(0.,1.,0.));
#3889=DIRECTION('ref_axis',(1.,0.,0.));
#3890=DIRECTION('center_axis',(0.,1.,0.));
#3891=DIRECTION('ref_axis',(1.,0.,0.));
#3892=DIRECTION('center_axis',(0.,1.,0.));
#3893=DIRECTION('ref_axis',(0.,0.,1.));
#3894=DIRECTION('center_axis',(0.,-1.,0.));
#3895=DIRECTION('ref_axis',(1.,0.,0.));
#3896=DIRECTION('center_axis',(0.,-1.,0.));
#3897=DIRECTION('ref_axis',(1.,0.,0.));
#3898=DIRECTION('center_axis',(0.,-1.,0.));
#3899=DIRECTION('ref_axis',(1.,0.,0.));
#3900=DIRECTION('',(0.707106781186547,0.707106781186548,8.65956056235493E-17));
#3901=DIRECTION('center_axis',(0.,-1.,0.));
#3902=DIRECTION('ref_axis',(1.,0.,0.));
#3903=DIRECTION('center_axis',(0.,-1.,0.));
#3904=DIRECTION('ref_axis',(1.,0.,0.));
#3905=DIRECTION('',(0.,1.,0.));
#3906=DIRECTION('center_axis',(0.,1.,0.));
#3907=DIRECTION('ref_axis',(1.,0.,0.));
#3908=DIRECTION('center_axis',(0.,-1.,0.));
#3909=DIRECTION('ref_axis',(1.,0.,0.));
#3910=DIRECTION('',(-0.707106781186547,0.707106781186548,-8.65956056235493E-17));
#3911=DIRECTION('center_axis',(0.,-1.,0.));
#3912=DIRECTION('ref_axis',(0.,0.,-1.));
#3913=DIRECTION('center_axis',(0.,-1.,0.));
#3914=DIRECTION('ref_axis',(1.,0.,0.));
#3915=DIRECTION('center_axis',(0.,1.,0.));
#3916=DIRECTION('ref_axis',(1.,0.,0.));
#3917=DIRECTION('center_axis',(0.,1.,0.));
#3918=DIRECTION('ref_axis',(1.,0.,0.));
#3919=DIRECTION('',(-0.447213595499958,0.894427190999916,-5.47678698264203E-17));
#3920=DIRECTION('center_axis',(0.,-1.,0.));
#3921=DIRECTION('ref_axis',(1.,0.,0.));
#3922=DIRECTION('',(0.,1.,0.));
#3923=DIRECTION('axis',(0.,0.,1.));
#3924=DIRECTION('refdir',(1.,0.,0.));
#3925=DIRECTION('center_axis',(0.,1.,0.));
#3926=DIRECTION('ref_axis',(1.,0.,0.));
#3927=DIRECTION('center_axis',(0.,-1.,0.));
#3928=DIRECTION('ref_axis',(1.,0.,0.));
#3929=DIRECTION('',(0.,-1.,0.));
#3930=DIRECTION('center_axis',(0.,-1.,0.));
#3931=DIRECTION('ref_axis',(1.,0.,0.));
#3932=DIRECTION('center_axis',(0.,1.,0.));
#3933=DIRECTION('ref_axis',(1.,0.,0.));
#3934=DIRECTION('center_axis',(0.,1.,0.));
#3935=DIRECTION('ref_axis',(1.,0.,0.));
#3936=DIRECTION('',(0.,-1.,0.));
#3937=DIRECTION('center_axis',(0.,1.,0.));
#3938=DIRECTION('ref_axis',(1.,0.,0.));
#3939=DIRECTION('center_axis',(0.,1.,0.));
#3940=DIRECTION('ref_axis',(1.,0.,0.));
#3941=DIRECTION('center_axis',(0.,1.,0.));
#3942=DIRECTION('ref_axis',(1.,0.,0.));
#3943=DIRECTION('axis',(0.,0.,1.));
#3944=DIRECTION('refdir',(1.,0.,0.));
#3945=DIRECTION('center_axis',(0.,-1.,0.));
#3946=DIRECTION('ref_axis',(1.,0.,0.));
#3947=DIRECTION('center_axis',(0.,1.,0.));
#3948=DIRECTION('ref_axis',(1.,0.,0.));
#3949=DIRECTION('',(0.,1.,0.));
#3950=DIRECTION('center_axis',(0.,-1.,0.));
#3951=DIRECTION('ref_axis',(1.,0.,0.));
#3952=DIRECTION('center_axis',(0.,1.,0.));
#3953=DIRECTION('ref_axis',(1.,0.,0.));
#3954=DIRECTION('center_axis',(0.,-1.,0.));
#3955=DIRECTION('ref_axis',(1.,0.,0.));
#3956=DIRECTION('',(-0.707106781186547,0.707106781186548,-8.65956056235493E-17));
#3957=DIRECTION('center_axis',(0.,-1.,0.));
#3958=DIRECTION('ref_axis',(0.,0.,-1.));
#3959=DIRECTION('center_axis',(0.,-1.,0.));
#3960=DIRECTION('ref_axis',(1.,0.,0.));
#3961=DIRECTION('center_axis',(0.,1.,0.));
#3962=DIRECTION('ref_axis',(1.,0.,0.));
#3963=DIRECTION('',(-0.866025403784439,-0.5,-1.06057523872491E-16));
#3964=DIRECTION('center_axis',(1.92296268638356E-16,0.,-1.));
#3965=DIRECTION('ref_axis',(-1.,0.,-1.92296268638356E-16));
#3966=DIRECTION('',(0.,1.,0.));
#3967=DIRECTION('',(-1.,0.,-1.92296268638356E-16));
#3968=DIRECTION('',(0.,1.,0.));
#3969=DIRECTION('center_axis',(0.866025403784439,0.,-0.5));
#3970=DIRECTION('ref_axis',(-0.5,0.,-0.866025403784439));
#3971=DIRECTION('',(0.,1.,0.));
#3972=DIRECTION('',(-0.5,0.,-0.866025403784439));
#3973=DIRECTION('center_axis',(0.866025403784439,0.,0.5));
#3974=DIRECTION('ref_axis',(0.5,0.,-0.866025403784439));
#3975=DIRECTION('',(0.,1.,0.));
#3976=DIRECTION('',(0.5,0.,-0.866025403784439));
#3977=DIRECTION('center_axis',(-1.92296268638356E-16,0.,1.));
#3978=DIRECTION('ref_axis',(1.,0.,1.92296268638356E-16));
#3979=DIRECTION('',(0.,1.,0.));
#3980=DIRECTION('',(1.,0.,1.92296268638356E-16));
#3981=DIRECTION('center_axis',(-0.866025403784439,0.,0.5));
#3982=DIRECTION('ref_axis',(0.5,0.,0.866025403784439));
#3983=DIRECTION('',(0.,1.,0.));
#3984=DIRECTION('',(0.5,0.,0.866025403784439));
#3985=DIRECTION('center_axis',(-0.866025403784439,0.,-0.5));
#3986=DIRECTION('ref_axis',(-0.5,0.,0.866025403784439));
#3987=DIRECTION('',(-0.5,0.,0.866025403784438));
#3988=DIRECTION('center_axis',(0.,1.,0.));
#3989=DIRECTION('ref_axis',(0.,0.,1.));
#3990=DIRECTION('center_axis',(0.,1.,0.));
#3991=DIRECTION('ref_axis',(1.,0.,0.));
#3992=DIRECTION('axis',(0.,0.,1.));
#3993=DIRECTION('refdir',(1.,0.,0.));
#3994=DIRECTION('center_axis',(0.,1.,0.));
#3995=DIRECTION('ref_axis',(1.,0.,0.));
#3996=DIRECTION('',(0.866025403784439,-0.5,1.06057523872491E-16));
#3997=DIRECTION('center_axis',(0.,-1.,0.));
#3998=DIRECTION('ref_axis',(1.,0.,0.));
#3999=DIRECTION('center_axis',(0.,-1.,0.));
#4000=DIRECTION('ref_axis',(1.,0.,0.));
#4001=DIRECTION('center_axis',(0.,1.,0.));
#4002=DIRECTION('ref_axis',(1.,0.,0.));
#4003=DIRECTION('',(-0.866025403784439,-0.5,-1.06057523872491E-16));
#4004=DIRECTION('center_axis',(1.92296268638356E-16,0.,-1.));
#4005=DIRECTION('ref_axis',(-1.,0.,-1.92296268638356E-16));
#4006=DIRECTION('',(0.,1.,0.));
#4007=DIRECTION('',(0.,1.,0.));
#4008=DIRECTION('center_axis',(-0.866025403784439,0.,-0.5));
#4009=DIRECTION('ref_axis',(-0.5,0.,0.866025403784439));
#4010=DIRECTION('',(0.,1.,0.));
#4011=DIRECTION('center_axis',(-0.866025403784439,0.,0.5));
#4012=DIRECTION('ref_axis',(0.5,0.,0.866025403784439));
#4013=DIRECTION('',(0.,1.,0.));
#4014=DIRECTION('center_axis',(0.,1.,0.));
#4015=DIRECTION('ref_axis',(1.,0.,0.));
#4016=DIRECTION('center_axis',(0.,1.,0.));
#4017=DIRECTION('ref_axis',(1.,0.,0.));
#4018=DIRECTION('',(0.,-1.,0.));
#4019=DIRECTION('center_axis',(0.,1.,0.));
#4020=DIRECTION('ref_axis',(1.,0.,0.));
#4021=DIRECTION('center_axis',(-1.92296268638356E-16,0.,1.));
#4022=DIRECTION('ref_axis',(1.,0.,1.92296268638356E-16));
#4023=DIRECTION('',(0.,1.,0.));
#4024=DIRECTION('center_axis',(0.866025403784439,0.,-0.5));
#4025=DIRECTION('ref_axis',(-0.5,0.,-0.866025403784439));
#4026=DIRECTION('',(0.,1.,0.));
#4027=DIRECTION('center_axis',(0.866025403784439,0.,0.5));
#4028=DIRECTION('ref_axis',(0.5,0.,-0.866025403784439));
#4029=DIRECTION('center_axis',(0.,1.,0.));
#4030=DIRECTION('ref_axis',(1.,0.,0.));
#4031=DIRECTION('center_axis',(0.,1.,0.));
#4032=DIRECTION('ref_axis',(1.,0.,0.));
#4033=DIRECTION('',(0.,0.,1.));
#4034=DIRECTION('',(1.,0.,0.));
#4035=DIRECTION('',(0.,0.,1.));
#4036=DIRECTION('',(1.,0.,0.));
#4037=DIRECTION('',(0.,0.,1.));
#4038=DIRECTION('',(1.,0.,0.));
#4039=DIRECTION('',(0.,0.,1.));
#4040=DIRECTION('',(1.,0.,0.));
#4041=DIRECTION('',(0.,0.,1.));
#4042=DIRECTION('',(1.,0.,0.));
#4043=DIRECTION('',(0.,0.,1.));
#4044=DIRECTION('',(1.,0.,0.));
#4045=DIRECTION('',(0.,0.,1.));
#4046=DIRECTION('',(1.,0.,0.));
#4047=DIRECTION('',(0.,0.,1.));
#4048=DIRECTION('',(1.,0.,0.));
#4049=DIRECTION('',(0.,0.,1.));
#4050=DIRECTION('',(1.,0.,0.));
#4051=DIRECTION('',(0.,0.,1.));
#4052=DIRECTION('',(1.,0.,0.));
#4053=DIRECTION('axis',(0.,0.,1.));
#4054=DIRECTION('refdir',(1.,0.,0.));
#4055=DIRECTION('axis',(0.,0.,1.));
#4056=DIRECTION('refdir',(1.,0.,0.));
#4057=DIRECTION('center_axis',(0.,1.,0.));
#4058=DIRECTION('ref_axis',(1.,0.,0.));
#4059=DIRECTION('center_axis',(0.,1.,0.));
#4060=DIRECTION('ref_axis',(1.,0.,0.));
#4061=DIRECTION('',(0.,1.,0.));
#4062=DIRECTION('center_axis',(0.,-1.,0.));
#4063=DIRECTION('ref_axis',(1.,0.,0.));
#4064=DIRECTION('center_axis',(0.,1.,0.));
#4065=DIRECTION('ref_axis',(1.,0.,0.));
#4066=DIRECTION('center_axis',(0.,1.,0.));
#4067=DIRECTION('ref_axis',(1.,0.,0.));
#4068=DIRECTION('center_axis',(0.,1.,0.));
#4069=DIRECTION('ref_axis',(1.,0.,0.));
#4070=DIRECTION('center_axis',(0.,1.,0.));
#4071=DIRECTION('ref_axis',(1.,0.,0.));
#4072=DIRECTION('',(0.,1.,0.));
#4073=DIRECTION('center_axis',(0.,1.,0.));
#4074=DIRECTION('ref_axis',(1.,0.,0.));
#4075=DIRECTION('center_axis',(0.,1.,0.));
#4076=DIRECTION('ref_axis',(1.,0.,0.));
#4077=DIRECTION('center_axis',(0.,-1.,0.));
#4078=DIRECTION('ref_axis',(1.,0.,0.));
#4079=DIRECTION('center_axis',(0.,1.,0.));
#4080=DIRECTION('ref_axis',(1.,0.,0.));
#4081=DIRECTION('',(0.,1.,0.));
#4082=DIRECTION('center_axis',(0.,1.,0.));
#4083=DIRECTION('ref_axis',(1.,0.,0.));
#4084=DIRECTION('center_axis',(0.,1.,0.));
#4085=DIRECTION('ref_axis',(1.,0.,0.));
#4086=DIRECTION('',(0.,-1.,0.));
#4087=DIRECTION('center_axis',(0.,1.,0.));
#4088=DIRECTION('ref_axis',(1.,0.,0.));
#4089=DIRECTION('center_axis',(0.,1.,0.));
#4090=DIRECTION('ref_axis',(1.,0.,0.));
#4091=DIRECTION('center_axis',(0.,1.,0.));
#4092=DIRECTION('ref_axis',(1.,0.,0.));
#4093=DIRECTION('axis',(0.,0.,1.));
#4094=DIRECTION('refdir',(1.,0.,0.));
#4095=DIRECTION('axis',(0.,0.,1.));
#4096=DIRECTION('refdir',(1.,0.,0.));
#4097=DIRECTION('center_axis',(0.,-1.,0.));
#4098=DIRECTION('ref_axis',(0.,0.,-1.));
#4099=DIRECTION('center_axis',(0.,-1.,0.));
#4100=DIRECTION('ref_axis',(1.,0.,0.));
#4101=DIRECTION('center_axis',(0.,-1.,0.));
#4102=DIRECTION('ref_axis',(1.,0.,0.));
#4103=DIRECTION('center_axis',(1.,0.,1.22464679914735E-16));
#4104=DIRECTION('ref_axis',(-1.22464679914735E-16,0.,1.));
#4105=DIRECTION('center_axis',(0.,1.,0.));
#4106=DIRECTION('ref_axis',(1.,0.,0.));
#4107=DIRECTION('center_axis',(0.,1.,0.));
#4108=DIRECTION('ref_axis',(1.,0.,0.));
#4109=DIRECTION('center_axis',(0.,-1.,0.));
#4110=DIRECTION('ref_axis',(1.,0.,0.));
#4111=DIRECTION('',(0.,1.,0.));
#4112=DIRECTION('center_axis',(0.,-1.,0.));
#4113=DIRECTION('ref_axis',(1.,0.,0.));
#4114=DIRECTION('center_axis',(0.,-1.,0.));
#4115=DIRECTION('ref_axis',(1.,0.,0.));
#4116=DIRECTION('center_axis',(0.,-1.,0.));
#4117=DIRECTION('ref_axis',(1.,0.,0.));
#4118=DIRECTION('',(0.,1.,0.));
#4119=DIRECTION('center_axis',(0.,-1.,0.));
#4120=DIRECTION('ref_axis',(1.,0.,0.));
#4121=DIRECTION('center_axis',(0.,1.,0.));
#4122=DIRECTION('ref_axis',(1.,0.,0.));
#4123=DIRECTION('',(-0.707106781186548,0.707106781186547,-8.65956056235493E-17));
#4124=DIRECTION('center_axis',(0.,-1.,0.));
#4125=DIRECTION('ref_axis',(1.,0.,0.));
#4126=DIRECTION('center_axis',(0.,1.,0.));
#4127=DIRECTION('ref_axis',(0.,0.,1.));
#4128=DIRECTION('center_axis',(0.,-1.,0.));
#4129=DIRECTION('ref_axis',(1.,0.,0.));
#4130=DIRECTION('center_axis',(0.,-1.,0.));
#4131=DIRECTION('ref_axis',(1.,0.,0.));
#4132=DIRECTION('',(0.,1.,0.));
#4133=DIRECTION('center_axis',(0.,-1.,0.));
#4134=DIRECTION('ref_axis',(0.,0.,-1.));
#4135=DIRECTION('center_axis',(0.,-1.,0.));
#4136=DIRECTION('ref_axis',(1.,0.,0.));
#4137=DIRECTION('center_axis',(0.,-1.,0.));
#4138=DIRECTION('ref_axis',(1.,0.,0.));
#4139=DIRECTION('',(0.707106781186548,0.707106781186547,8.65956056235493E-17));
#4140=DIRECTION('axis',(0.,0.,1.));
#4141=DIRECTION('refdir',(1.,0.,0.));
#4142=DIRECTION('center_axis',(0.,-1.,0.));
#4143=DIRECTION('ref_axis',(0.,0.,-1.));
#4144=DIRECTION('center_axis',(0.,-1.,0.));
#4145=DIRECTION('ref_axis',(1.,0.,0.));
#4146=DIRECTION('center_axis',(0.,-1.,0.));
#4147=DIRECTION('ref_axis',(1.,0.,0.));
#4148=DIRECTION('center_axis',(1.,0.,1.22464679914735E-16));
#4149=DIRECTION('ref_axis',(-1.22464679914735E-16,0.,1.));
#4150=DIRECTION('center_axis',(0.,1.,0.));
#4151=DIRECTION('ref_axis',(1.,0.,0.));
#4152=DIRECTION('center_axis',(0.,1.,0.));
#4153=DIRECTION('ref_axis',(1.,0.,0.));
#4154=DIRECTION('center_axis',(0.,-1.,0.));
#4155=DIRECTION('ref_axis',(1.,0.,0.));
#4156=DIRECTION('center_axis',(0.,-1.,0.));
#4157=DIRECTION('ref_axis',(1.,0.,0.));
#4158=DIRECTION('',(0.,1.,0.));
#4159=DIRECTION('center_axis',(0.,1.,0.));
#4160=DIRECTION('ref_axis',(0.,0.,1.));
#4161=DIRECTION('center_axis',(0.,-1.,0.));
#4162=DIRECTION('ref_axis',(1.,0.,0.));
#4163=DIRECTION('center_axis',(0.,-1.,0.));
#4164=DIRECTION('ref_axis',(1.,0.,0.));
#4165=DIRECTION('center_axis',(0.,-1.,0.));
#4166=DIRECTION('ref_axis',(1.,0.,0.));
#4167=DIRECTION('center_axis',(0.,-1.,0.));
#4168=DIRECTION('ref_axis',(1.,0.,0.));
#4169=DIRECTION('',(0.707106781186548,0.707106781186547,8.65956056235494E-17));
#4170=DIRECTION('center_axis',(0.,-1.,0.));
#4171=DIRECTION('ref_axis',(1.,0.,0.));
#4172=DIRECTION('center_axis',(0.,-1.,0.));
#4173=DIRECTION('ref_axis',(1.,0.,0.));
#4174=DIRECTION('',(0.,1.,0.));
#4175=DIRECTION('center_axis',(0.,1.,0.));
#4176=DIRECTION('ref_axis',(1.,0.,0.));
#4177=DIRECTION('center_axis',(0.,-1.,0.));
#4178=DIRECTION('ref_axis',(1.,0.,0.));
#4179=DIRECTION('',(-0.707106781186548,0.707106781186547,-8.65956056235494E-17));
#4180=DIRECTION('center_axis',(0.,-1.,0.));
#4181=DIRECTION('ref_axis',(0.,0.,-1.));
#4182=DIRECTION('center_axis',(0.,-1.,0.));
#4183=DIRECTION('ref_axis',(1.,0.,0.));
#4184=DIRECTION('',(0.,1.,0.));
#4185=DIRECTION('axis',(0.,0.,1.));
#4186=DIRECTION('refdir',(1.,0.,0.));
#4187=DIRECTION('center_axis',(0.,0.,1.));
#4188=DIRECTION('ref_axis',(1.,0.,0.));
#4189=DIRECTION('center_axis',(1.22464679914735E-16,-1.,0.));
#4190=DIRECTION('ref_axis',(-1.,-1.22464679914735E-16,0.));
#4191=DIRECTION('center_axis',(0.78183148246803,0.,0.623489801858733));
#4192=DIRECTION('ref_axis',(0.623489801858734,0.,-0.78183148246803));
#4193=DIRECTION('center_axis',(7.63554790147315E-17,-1.,-9.57467422477103E-17));
#4194=DIRECTION('ref_axis',(-0.623489801858734,-1.22464679914735E-16,0.78183148246803));
#4195=DIRECTION('center_axis',(0.974927912181824,0.,-0.222520933956314));
#4196=DIRECTION('ref_axis',(-0.222520933956314,0.,-0.974927912181824));
#4197=DIRECTION('center_axis',(-2.7250954951288E-17,-1.,-1.19394234705288E-16));
#4198=DIRECTION('ref_axis',(0.222520933956314,-1.22464679914735E-16,0.974927912181824));
#4199=DIRECTION('center_axis',(0.433883739117558,0.,-0.900968867902419));
#4200=DIRECTION('ref_axis',(-0.900968867902419,0.,-0.433883739117558));
#4201=DIRECTION('center_axis',(-1.10336864020811E-16,-1.,-5.31354332312403E-17));
#4202=DIRECTION('ref_axis',(0.900968867902419,-1.22464679914735E-16,0.433883739117558));
#4203=DIRECTION('center_axis',(-0.433883739117558,0.,-0.900968867902419));
#4204=DIRECTION('ref_axis',(-0.900968867902419,0.,0.433883739117558));
#4205=DIRECTION('center_axis',(-1.10336864020811E-16,-1.,5.31354332312403E-17));
#4206=DIRECTION('ref_axis',(0.900968867902419,-1.22464679914735E-16,-0.433883739117558));
#4207=DIRECTION('center_axis',(-0.974927912181824,0.,-0.222520933956314));
#4208=DIRECTION('ref_axis',(-0.222520933956315,0.,0.974927912181824));
#4209=DIRECTION('center_axis',(-2.7250954951288E-17,-1.,1.19394234705288E-16));
#4210=DIRECTION('ref_axis',(0.222520933956315,-1.22464679914735E-16,-0.974927912181824));
#4211=DIRECTION('center_axis',(-0.78183148246803,0.,0.623489801858734));
#4212=DIRECTION('ref_axis',(0.623489801858733,0.,0.78183148246803));
#4213=DIRECTION('center_axis',(7.63554790147315E-17,-1.,9.57467422477103E-17));
#4214=DIRECTION('ref_axis',(-0.623489801858733,-1.22464679914735E-16,-0.78183148246803));
#4215=DIRECTION('axis',(0.,0.,1.));
#4216=DIRECTION('refdir',(1.,0.,0.));
#4217=DIRECTION('center_axis',(0.,0.,1.));
#4218=DIRECTION('ref_axis',(1.,0.,0.));
#4219=DIRECTION('center_axis',(0.,-1.,0.));
#4220=DIRECTION('ref_axis',(0.,0.,-1.));
#4221=DIRECTION('center_axis',(0.,-1.,0.));
#4222=DIRECTION('ref_axis',(0.,0.,-1.));
#4223=DIRECTION('center_axis',(0.,1.,0.));
#4224=DIRECTION('ref_axis',(1.,0.,0.));
#4225=DIRECTION('center_axis',(0.,1.,0.));
#4226=DIRECTION('ref_axis',(1.,0.,0.));
#4227=DIRECTION('center_axis',(0.,1.,0.));
#4228=DIRECTION('ref_axis',(1.,0.,0.));
#4229=DIRECTION('center_axis',(0.,1.,0.));
#4230=DIRECTION('ref_axis',(1.,0.,0.));
#4231=DIRECTION('',(0.,-1.,0.));
#4232=DIRECTION('center_axis',(0.,-1.,0.));
#4233=DIRECTION('ref_axis',(1.,0.,0.));
#4234=DIRECTION('center_axis',(0.,1.,0.));
#4235=DIRECTION('ref_axis',(1.,0.,0.));
#4236=DIRECTION('center_axis',(0.,1.,0.));
#4237=DIRECTION('ref_axis',(1.,0.,0.));
#4238=DIRECTION('center_axis',(0.,1.,0.));
#4239=DIRECTION('ref_axis',(1.,0.,0.));
#4240=DIRECTION('center_axis',(0.,1.,0.));
#4241=DIRECTION('ref_axis',(1.,0.,0.));
#4242=DIRECTION('center_axis',(0.,1.,0.));
#4243=DIRECTION('ref_axis',(1.,0.,0.));
#4244=DIRECTION('center_axis',(0.,1.,0.));
#4245=DIRECTION('ref_axis',(1.,0.,0.));
#4246=DIRECTION('center_axis',(0.,-1.,0.));
#4247=DIRECTION('ref_axis',(1.,0.,0.));
#4248=DIRECTION('center_axis',(0.,-1.,0.));
#4249=DIRECTION('ref_axis',(0.,0.,-1.));
#4250=DIRECTION('center_axis',(8.96625347776458E-17,0.,1.));
#4251=DIRECTION('ref_axis',(1.,0.,0.));
#4252=DIRECTION('center_axis',(0.,-1.,0.));
#4253=DIRECTION('ref_axis',(0.,0.,-1.));
#4254=DIRECTION('center_axis',(0.,1.,0.));
#4255=DIRECTION('ref_axis',(1.,0.,0.));
#4256=DIRECTION('center_axis',(0.,-1.,0.));
#4257=DIRECTION('ref_axis',(1.,0.,0.));
#4258=DIRECTION('center_axis',(0.,-1.,0.));
#4259=DIRECTION('ref_axis',(0.,0.,-1.));
#4260=DIRECTION('center_axis',(0.,0.,1.));
#4261=DIRECTION('ref_axis',(1.,0.,0.));
#4262=DIRECTION('center_axis',(0.,-1.,0.));
#4263=DIRECTION('ref_axis',(0.,0.,-1.));
#4264=DIRECTION('center_axis',(0.,1.,0.));
#4265=DIRECTION('ref_axis',(1.,0.,0.));
#4266=DIRECTION('center_axis',(0.,-1.,0.));
#4267=DIRECTION('ref_axis',(1.,0.,0.));
#4268=DIRECTION('center_axis',(0.,-1.,0.));
#4269=DIRECTION('ref_axis',(1.,0.,0.));
#4270=DIRECTION('center_axis',(0.,-1.,0.));
#4271=DIRECTION('ref_axis',(0.,0.,-1.));
#4272=DIRECTION('center_axis',(0.,0.,1.));
#4273=DIRECTION('ref_axis',(1.,0.,0.));
#4274=DIRECTION('center_axis',(0.,-1.,0.));
#4275=DIRECTION('ref_axis',(0.,0.,-1.));
#4276=DIRECTION('center_axis',(0.,1.,0.));
#4277=DIRECTION('ref_axis',(1.,0.,0.));
#4278=DIRECTION('center_axis',(0.,-1.,0.));
#4279=DIRECTION('ref_axis',(1.,0.,0.));
#4280=DIRECTION('center_axis',(0.,-1.,0.));
#4281=DIRECTION('ref_axis',(0.,0.,-1.));
#4282=DIRECTION('center_axis',(8.96625347776458E-17,0.,1.));
#4283=DIRECTION('ref_axis',(1.,0.,0.));
#4284=DIRECTION('center_axis',(0.,-1.,0.));
#4285=DIRECTION('ref_axis',(0.,0.,-1.));
#4286=DIRECTION('center_axis',(0.,1.,0.));
#4287=DIRECTION('ref_axis',(1.,0.,0.));
#4288=DIRECTION('center_axis',(0.,-1.,0.));
#4289=DIRECTION('ref_axis',(1.,0.,0.));
#4290=DIRECTION('center_axis',(0.,-1.,0.));
#4291=DIRECTION('ref_axis',(0.,0.,-1.));
#4292=DIRECTION('center_axis',(0.,0.,1.));
#4293=DIRECTION('ref_axis',(1.,0.,0.));
#4294=DIRECTION('center_axis',(0.,-1.,0.));
#4295=DIRECTION('ref_axis',(0.,0.,-1.));
#4296=DIRECTION('center_axis',(0.,1.,0.));
#4297=DIRECTION('ref_axis',(1.,0.,0.));
#4298=DIRECTION('center_axis',(0.,1.,0.));
#4299=DIRECTION('ref_axis',(1.,0.,0.));
#4300=DIRECTION('',(0.,1.,0.));
#4301=DIRECTION('center_axis',(0.,-1.,0.));
#4302=DIRECTION('ref_axis',(1.,0.,0.));
#4303=DIRECTION('center_axis',(0.,-1.,0.));
#4304=DIRECTION('ref_axis',(1.,0.,0.));
#4305=DIRECTION('center_axis',(0.,1.,0.));
#4306=DIRECTION('ref_axis',(1.,0.,0.));
#4307=DIRECTION('center_axis',(0.,-1.,0.));
#4308=DIRECTION('ref_axis',(0.,0.,-1.));
#4309=DIRECTION('center_axis',(0.,0.,1.));
#4310=DIRECTION('ref_axis',(1.,0.,0.));
#4311=DIRECTION('center_axis',(0.,-1.,0.));
#4312=DIRECTION('ref_axis',(0.,0.,-1.));
#4313=DIRECTION('center_axis',(0.,-1.,0.));
#4314=DIRECTION('ref_axis',(-1.,0.,0.));
#4315=DIRECTION('center_axis',(0.,1.,0.));
#4316=DIRECTION('ref_axis',(1.,0.,0.));
#4317=DIRECTION('axis',(0.,0.,1.));
#4318=DIRECTION('refdir',(1.,0.,0.));
#4319=DIRECTION('center_axis',(0.,1.,0.));
#4320=DIRECTION('ref_axis',(0.,0.,1.));
#4321=DIRECTION('center_axis',(0.,-1.,0.));
#4322=DIRECTION('ref_axis',(1.,0.,0.));
#4323=DIRECTION('center_axis',(0.,-1.,0.));
#4324=DIRECTION('ref_axis',(1.,0.,0.));
#4325=DIRECTION('center_axis',(0.,-1.,0.));
#4326=DIRECTION('ref_axis',(1.,0.,0.));
#4327=DIRECTION('center_axis',(0.,-1.,0.));
#4328=DIRECTION('ref_axis',(1.,0.,0.));
#4329=DIRECTION('',(0.,1.,0.));
#4330=DIRECTION('center_axis',(0.,-1.,0.));
#4331=DIRECTION('ref_axis',(0.,0.,-1.));
#4332=DIRECTION('center_axis',(0.,-1.,0.));
#4333=DIRECTION('ref_axis',(1.,0.,0.));
#4334=DIRECTION('center_axis',(0.,-1.,0.));
#4335=DIRECTION('ref_axis',(1.,0.,0.));
#4336=DIRECTION('',(0.,1.,0.));
#4337=DIRECTION('center_axis',(0.,1.,0.));
#4338=DIRECTION('ref_axis',(0.,0.,1.));
#4339=DIRECTION('center_axis',(0.,-1.,0.));
#4340=DIRECTION('ref_axis',(1.,0.,0.));
#4341=DIRECTION('center_axis',(0.,-1.,0.));
#4342=DIRECTION('ref_axis',(1.,0.,0.));
#4343=DIRECTION('center_axis',(0.,-1.,0.));
#4344=DIRECTION('ref_axis',(1.,0.,0.));
#4345=DIRECTION('center_axis',(0.,-1.,0.));
#4346=DIRECTION('ref_axis',(1.,0.,0.));
#4347=DIRECTION('',(0.,1.,0.));
#4348=DIRECTION('center_axis',(0.,-1.,0.));
#4349=DIRECTION('ref_axis',(0.,0.,-1.));
#4350=DIRECTION('center_axis',(0.,-1.,0.));
#4351=DIRECTION('ref_axis',(1.,0.,0.));
#4352=DIRECTION('center_axis',(0.,-1.,0.));
#4353=DIRECTION('ref_axis',(1.,0.,0.));
#4354=DIRECTION('',(0.,1.,0.));
#4355=DIRECTION('',(0.,0.,1.));
#4356=DIRECTION('',(1.,0.,0.));
#4357=DIRECTION('',(0.,0.,1.));
#4358=DIRECTION('',(1.,0.,0.));
#4359=DIRECTION('',(0.,0.,1.));
#4360=DIRECTION('',(1.,0.,0.));
#4361=DIRECTION('',(0.,0.,1.));
#4362=DIRECTION('',(1.,0.,0.));
#4363=DIRECTION('',(0.,0.,1.));
#4364=DIRECTION('',(1.,0.,0.));
#4365=DIRECTION('axis',(0.,0.,1.));
#4366=DIRECTION('refdir',(1.,0.,0.));
#4367=DIRECTION('center_axis',(0.,1.,0.));
#4368=DIRECTION('ref_axis',(1.,0.,0.));
#4369=DIRECTION('center_axis',(0.,-1.,0.));
#4370=DIRECTION('ref_axis',(1.,0.,0.));
#4371=DIRECTION('',(0.,-1.,0.));
#4372=DIRECTION('center_axis',(0.,-1.,0.));
#4373=DIRECTION('ref_axis',(1.,0.,0.));
#4374=DIRECTION('center_axis',(0.,1.,0.));
#4375=DIRECTION('ref_axis',(1.,0.,0.));
#4376=DIRECTION('center_axis',(0.,1.,0.));
#4377=DIRECTION('ref_axis',(1.,0.,0.));
#4378=DIRECTION('',(0.,-1.,0.));
#4379=DIRECTION('center_axis',(0.,1.,0.));
#4380=DIRECTION('ref_axis',(1.,0.,0.));
#4381=DIRECTION('center_axis',(0.,1.,0.));
#4382=DIRECTION('ref_axis',(1.,0.,0.));
#4383=DIRECTION('center_axis',(0.,1.,0.));
#4384=DIRECTION('ref_axis',(1.,0.,0.));
#4385=DIRECTION('',(0.,0.,1.));
#4386=DIRECTION('',(1.,0.,0.));
#4387=DIRECTION('',(0.,0.,1.));
#4388=DIRECTION('',(1.,0.,0.));
#4389=DIRECTION('',(0.,0.,1.));
#4390=DIRECTION('',(1.,0.,0.));
#4391=DIRECTION('',(0.,0.,1.));
#4392=DIRECTION('',(1.,0.,0.));
#4393=DIRECTION('',(0.,0.,1.));
#4394=DIRECTION('',(1.,0.,0.));
#4395=DIRECTION('axis',(0.,0.,1.));
#4396=DIRECTION('refdir',(1.,0.,0.));
#4397=DIRECTION('axis',(0.,0.,1.));
#4398=DIRECTION('refdir',(1.,0.,0.));
#4399=DIRECTION('center_axis',(0.,1.,0.));
#4400=DIRECTION('ref_axis',(1.,0.,0.));
#4401=DIRECTION('center_axis',(0.,1.,0.));
#4402=DIRECTION('ref_axis',(1.,0.,0.));
#4403=DIRECTION('',(0.,1.,0.));
#4404=DIRECTION('center_axis',(0.,-1.,0.));
#4405=DIRECTION('ref_axis',(1.,0.,0.));
#4406=DIRECTION('center_axis',(-0.196116135138184,0.,0.98058067569092));
#4407=DIRECTION('ref_axis',(0.98058067569092,0.,0.196116135138184));
#4408=DIRECTION('',(0.,-1.,0.));
#4409=DIRECTION('',(0.98058067569092,0.,0.196116135138184));
#4410=DIRECTION('',(0.,1.,0.));
#4411=DIRECTION('',(-0.98058067569092,0.,-0.196116135138184));
#4412=DIRECTION('center_axis',(-1.,0.,0.));
#4413=DIRECTION('ref_axis',(0.,0.,1.));
#4414=DIRECTION('',(0.,0.,-1.));
#4415=DIRECTION('',(0.,0.,1.));
#4416=DIRECTION('',(0.,1.,0.));
#4417=DIRECTION('center_axis',(0.196116135138184,0.,-0.98058067569092));
#4418=DIRECTION('ref_axis',(-0.98058067569092,0.,-0.196116135138184));
#4419=DIRECTION('',(0.,1.,0.));
#4420=DIRECTION('',(0.98058067569092,0.,0.196116135138184));
#4421=DIRECTION('',(-0.98058067569092,0.,-0.196116135138184));
#4422=DIRECTION('center_axis',(0.,1.,0.));
#4423=DIRECTION('ref_axis',(1.,0.,0.));
#4424=DIRECTION('center_axis',(0.,1.,0.));
#4425=DIRECTION('ref_axis',(1.,0.,0.));
#4426=DIRECTION('',(1.,0.,0.));
#4427=DIRECTION('',(0.,0.,1.));
#4428=DIRECTION('',(-1.,0.,0.));
#4429=DIRECTION('',(0.,0.,-1.));
#4430=DIRECTION('center_axis',(0.,1.,0.));
#4431=DIRECTION('ref_axis',(1.,0.,0.));
#4432=DIRECTION('center_axis',(0.,1.,0.));
#4433=DIRECTION('ref_axis',(1.,0.,0.));
#4434=DIRECTION('center_axis',(0.,1.,0.));
#4435=DIRECTION('ref_axis',(1.,0.,0.));
#4436=DIRECTION('',(0.,-1.,0.));
#4437=DIRECTION('center_axis',(-1.,0.,0.));
#4438=DIRECTION('ref_axis',(0.,0.,1.));
#4439=DIRECTION('',(0.,1.,0.));
#4440=DIRECTION('',(0.,1.,0.));
#4441=DIRECTION('',(0.,0.,1.));
#4442=DIRECTION('center_axis',(0.,0.,-1.));
#4443=DIRECTION('ref_axis',(-1.,0.,0.));
#4444=DIRECTION('',(-1.,0.,0.));
#4445=DIRECTION('',(0.,1.,0.));
#4446=DIRECTION('center_axis',(1.,0.,0.));
#4447=DIRECTION('ref_axis',(0.,0.,-1.));
#4448=DIRECTION('',(0.,0.,-1.));
#4449=DIRECTION('',(0.,1.,0.));
#4450=DIRECTION('center_axis',(0.,0.,1.));
#4451=DIRECTION('ref_axis',(1.,0.,0.));
#4452=DIRECTION('',(1.,0.,0.));
#4453=DIRECTION('center_axis',(0.,1.,0.));
#4454=DIRECTION('ref_axis',(1.,0.,0.));
#4455=DIRECTION('center_axis',(0.,1.,0.));
#4456=DIRECTION('ref_axis',(1.,0.,0.));
#4457=DIRECTION('center_axis',(0.,1.,0.));
#4458=DIRECTION('ref_axis',(1.,0.,0.));
#4459=DIRECTION('axis',(0.,0.,1.));
#4460=DIRECTION('refdir',(1.,0.,0.));
#4461=DIRECTION('center_axis',(0.,1.,0.));
#4462=DIRECTION('ref_axis',(-1.,0.,0.));
#4463=DIRECTION('',(-1.,0.,0.));
#4464=DIRECTION('',(0.,0.,1.));
#4465=DIRECTION('',(-1.,0.,0.));
#4466=DIRECTION('',(0.,0.,1.));
#4467=DIRECTION('center_axis',(1.,0.,0.));
#4468=DIRECTION('ref_axis',(0.,1.,0.));
#4469=DIRECTION('',(0.,1.,0.));
#4470=DIRECTION('',(0.,1.,0.));
#4471=DIRECTION('',(0.,0.,1.));
#4472=DIRECTION('center_axis',(0.,-1.,0.));
#4473=DIRECTION('ref_axis',(1.,0.,0.));
#4474=DIRECTION('',(1.,0.,0.));
#4475=DIRECTION('',(1.,0.,0.));
#4476=DIRECTION('',(0.,0.,1.));
#4477=DIRECTION('center_axis',(-1.,0.,0.));
#4478=DIRECTION('ref_axis',(0.,-1.,0.));
#4479=DIRECTION('',(0.,-1.,0.));
#4480=DIRECTION('',(0.,-1.,0.));
#4481=DIRECTION('center_axis',(0.,0.,1.));
#4482=DIRECTION('ref_axis',(1.,0.,0.));
#4483=DIRECTION('center_axis',(0.,0.,1.));
#4484=DIRECTION('ref_axis',(1.,0.,0.));
#4485=DIRECTION('',(0.,0.,1.));
#4486=DIRECTION('',(1.,0.,0.));
#4487=DIRECTION('',(0.,0.,1.));
#4488=DIRECTION('',(1.,0.,0.));
#4489=DIRECTION('',(0.,0.,1.));
#4490=DIRECTION('',(1.,0.,0.));
#4491=DIRECTION('',(0.,0.,1.));
#4492=DIRECTION('',(1.,0.,0.));
#4493=DIRECTION('',(0.,0.,1.));
#4494=DIRECTION('',(1.,0.,0.));
#4495=CARTESIAN_POINT('',(0.,0.,0.));
#4496=CARTESIAN_POINT('',(0.,0.,0.));
#4497=CARTESIAN_POINT('',(0.,0.,0.));
#4498=CARTESIAN_POINT('Origin',(-4.,0.64,9.9));
#4499=CARTESIAN_POINT('',(-4.,-0.64,10.8));
#4500=CARTESIAN_POINT('',(-4.,0.64,10.8));
#4501=CARTESIAN_POINT('',(-4.,0.32,10.8));
#4502=CARTESIAN_POINT('',(-4.,-0.64,10.));
#4503=CARTESIAN_POINT('',(-4.,-0.64,9.9));
#4504=CARTESIAN_POINT('',(-4.,0.64,10.));
#4505=CARTESIAN_POINT('',(-4.,0.32,10.));
#4506=CARTESIAN_POINT('',(-4.,0.64,9.9));
#4507=CARTESIAN_POINT('Origin',(-4.,-0.64,9.9));
#4508=CARTESIAN_POINT('',(1.2,-0.64,10.8));
#4509=CARTESIAN_POINT('',(-2.,-0.64,10.8));
#4510=CARTESIAN_POINT('',(1.2,-0.64,10.));
#4511=CARTESIAN_POINT('',(1.2,-0.64,9.9));
#4512=CARTESIAN_POINT('',(-2.4,-0.64,10.));
#4513=CARTESIAN_POINT('',(-2.,-0.64,10.));
#4514=CARTESIAN_POINT('',(-2.4,-0.64,9.9));
#4515=CARTESIAN_POINT('',(-2.4,-0.64,10.));
#4516=CARTESIAN_POINT('',(-3.6,-0.64,9.9));
#4517=CARTESIAN_POINT('',(-4.,-0.64,9.9));
#4518=CARTESIAN_POINT('',(-3.6,-0.64,10.));
#4519=CARTESIAN_POINT('',(-3.6,-0.64,9.15));
#4520=CARTESIAN_POINT('',(-2.,-0.64,10.));
#4521=CARTESIAN_POINT('Origin',(-1.4,0.,9.9));
#4522=CARTESIAN_POINT('',(-2.4,-0.62,9.9));
#4523=CARTESIAN_POINT('',(-2.4,-0.51,9.9));
#4524=CARTESIAN_POINT('',(-3.6,-0.62,9.9));
#4525=CARTESIAN_POINT('',(-2.2,-0.62,9.9));
#4526=CARTESIAN_POINT('',(-3.6,-0.51,9.9));
#4527=CARTESIAN_POINT('Origin',(-1.4,0.,9.9));
#4528=CARTESIAN_POINT('',(-2.4,0.64,9.9));
#4529=CARTESIAN_POINT('',(-2.4,0.62,9.9));
#4530=CARTESIAN_POINT('',(-2.4,0.31,9.9));
#4531=CARTESIAN_POINT('',(-3.6,0.64,9.9));
#4532=CARTESIAN_POINT('',(1.2,0.64,9.9));
#4533=CARTESIAN_POINT('',(-3.6,0.62,9.9));
#4534=CARTESIAN_POINT('',(-3.6,0.31,9.9));
#4535=CARTESIAN_POINT('',(-2.2,0.62,9.9));
#4536=CARTESIAN_POINT('Origin',(1.2,0.64,9.9));
#4537=CARTESIAN_POINT('',(1.2,0.64,10.8));
#4538=CARTESIAN_POINT('',(0.6,0.64,10.8));
#4539=CARTESIAN_POINT('',(-3.6,0.64,10.));
#4540=CARTESIAN_POINT('',(0.6,0.64,10.));
#4541=CARTESIAN_POINT('',(-3.6,0.64,9.15));
#4542=CARTESIAN_POINT('',(-2.4,0.64,10.));
#4543=CARTESIAN_POINT('',(-2.4,0.64,10.));
#4544=CARTESIAN_POINT('',(1.2,0.64,10.));
#4545=CARTESIAN_POINT('',(0.6,0.64,10.));
#4546=CARTESIAN_POINT('',(1.2,0.64,9.9));
#4547=CARTESIAN_POINT('Origin',(1.2,-0.64,9.9));
#4548=CARTESIAN_POINT('',(1.2,-0.32,10.8));
#4549=CARTESIAN_POINT('',(1.2,-0.32,10.));
#4550=CARTESIAN_POINT('Origin',(-3.,0.62,9.25));
#4551=CARTESIAN_POINT('',(-3.6,0.62,8.4));
#4552=CARTESIAN_POINT('',(-3.6,0.62,10.1));
#4553=CARTESIAN_POINT('',(-2.4,0.62,8.4));
#4554=CARTESIAN_POINT('',(-3.6,0.62,8.4));
#4555=CARTESIAN_POINT('',(-2.4,0.62,8.4));
#4556=CARTESIAN_POINT('',(-3.325,0.62,9.));
#4557=CARTESIAN_POINT('Origin',(-3.,0.62,9.));
#4558=CARTESIAN_POINT('Origin',(-3.6,0.62,8.4));
#4559=CARTESIAN_POINT('',(-3.6,1.02,10.));
#4560=CARTESIAN_POINT('',(-3.6,0.31,10.));
#4561=CARTESIAN_POINT('',(-3.6,1.02,8.4));
#4562=CARTESIAN_POINT('',(-3.6,1.02,10.1));
#4563=CARTESIAN_POINT('',(-3.6,0.62,8.4));
#4564=CARTESIAN_POINT('Origin',(-3.6,-1.02,8.4));
#4565=CARTESIAN_POINT('',(-3.6,-0.62,8.4));
#4566=CARTESIAN_POINT('',(-3.6,-0.62,10.1));
#4567=CARTESIAN_POINT('',(-3.6,-1.02,8.4));
#4568=CARTESIAN_POINT('',(-3.6,-1.02,8.4));
#4569=CARTESIAN_POINT('',(-3.6,-1.02,10.));
#4570=CARTESIAN_POINT('',(-3.6,-1.02,10.1));
#4571=CARTESIAN_POINT('',(-3.6,-0.51,10.));
#4572=CARTESIAN_POINT('Origin',(-3.,-1.1,9.));
#4573=CARTESIAN_POINT('',(-3.325,-1.02,9.));
#4574=CARTESIAN_POINT('Origin',(-3.,-1.02,9.));
#4575=CARTESIAN_POINT('',(-3.325,-0.62,9.));
#4576=CARTESIAN_POINT('',(-3.325,-1.1,9.));
#4577=CARTESIAN_POINT('Origin',(-3.,-0.62,9.));
#4578=CARTESIAN_POINT('Origin',(-3.,-1.1,9.));
#4579=CARTESIAN_POINT('',(-3.325,1.02,9.));
#4580=CARTESIAN_POINT('',(-3.325,-1.1,9.));
#4581=CARTESIAN_POINT('Origin',(-3.,1.02,9.));
#4582=CARTESIAN_POINT('Origin',(-3.,1.02,9.25));
#4583=CARTESIAN_POINT('',(-2.4,1.02,10.));
#4584=CARTESIAN_POINT('',(-1.5,1.02,10.));
#4585=CARTESIAN_POINT('',(-2.4,1.02,8.4));
#4586=CARTESIAN_POINT('',(-2.4,1.02,8.4));
#4587=CARTESIAN_POINT('',(-3.6,1.02,8.4));
#4588=CARTESIAN_POINT('Origin',(-2.4,0.62,10.1));
#4589=CARTESIAN_POINT('',(-2.4,0.62,8.4));
#4590=CARTESIAN_POINT('',(-2.4,0.31,10.));
#4591=CARTESIAN_POINT('Origin',(-2.4,0.62,8.4));
#4592=CARTESIAN_POINT('Origin',(-3.,-0.62,9.25));
#4593=CARTESIAN_POINT('',(-2.4,-0.62,8.4));
#4594=CARTESIAN_POINT('',(-2.4,-0.62,8.4));
#4595=CARTESIAN_POINT('',(-3.6,-0.62,8.4));
#4596=CARTESIAN_POINT('Origin',(-2.4,-1.02,10.1));
#4597=CARTESIAN_POINT('',(-2.4,-1.02,10.));
#4598=CARTESIAN_POINT('',(-2.4,-0.51,10.));
#4599=CARTESIAN_POINT('',(-2.4,-1.02,8.4));
#4600=CARTESIAN_POINT('',(-2.4,-1.02,8.4));
#4601=CARTESIAN_POINT('',(-2.4,-1.02,8.4));
#4602=CARTESIAN_POINT('Origin',(-2.4,-1.02,8.4));
#4603=CARTESIAN_POINT('',(-3.6,-1.02,8.4));
#4604=CARTESIAN_POINT('Origin',(-3.,-1.02,9.25));
#4605=CARTESIAN_POINT('',(-1.5,-1.02,10.));
#4606=CARTESIAN_POINT('Origin',(0.,-2.1,5.));
#4607=CARTESIAN_POINT('',(0.6,-1.5,5.));
#4608=CARTESIAN_POINT('',(-0.6,-1.5,5.));
#4609=CARTESIAN_POINT('Origin',(0.,-1.5,5.));
#4610=CARTESIAN_POINT('',(0.6,-2.,5.));
#4611=CARTESIAN_POINT('',(0.6,-2.1,5.));
#4612=CARTESIAN_POINT('',(-0.6,-2.,5.));
#4613=CARTESIAN_POINT('Origin',(0.,-2.,5.));
#4614=CARTESIAN_POINT('',(-0.6,-2.1,5.));
#4615=CARTESIAN_POINT('Origin',(0.,-2.1,5.));
#4616=CARTESIAN_POINT('',(0.6,2.,5.));
#4617=CARTESIAN_POINT('',(-0.6,2.,5.));
#4618=CARTESIAN_POINT('Origin',(0.,2.,5.));
#4619=CARTESIAN_POINT('',(0.6,1.5,5.));
#4620=CARTESIAN_POINT('',(0.6,-2.1,5.));
#4621=CARTESIAN_POINT('',(-0.6,1.5,5.));
#4622=CARTESIAN_POINT('Origin',(0.,1.5,5.));
#4623=CARTESIAN_POINT('',(-0.6,-2.1,5.));
#4624=CARTESIAN_POINT('Origin',(0.,1.5,7.55));
#4625=CARTESIAN_POINT('',(1.4,1.5,5.));
#4626=CARTESIAN_POINT('',(-1.4,1.5,5.));
#4627=CARTESIAN_POINT('',(1.4,1.5,10.));
#4628=CARTESIAN_POINT('',(1.4,1.5,5.));
#4629=CARTESIAN_POINT('',(-1.4,1.5,10.));
#4630=CARTESIAN_POINT('',(0.,1.5,10.));
#4631=CARTESIAN_POINT('',(-1.4,1.5,5.));
#4632=CARTESIAN_POINT('',(-1.4,1.5,10.1));
#4633=CARTESIAN_POINT('',(-1.4,1.5,5.));
#4634=CARTESIAN_POINT('Origin',(1.4,1.5,5.));
#4635=CARTESIAN_POINT('',(1.4,2.,5.));
#4636=CARTESIAN_POINT('',(-1.4,2.,5.));
#4637=CARTESIAN_POINT('',(1.4,1.5,5.));
#4638=CARTESIAN_POINT('Origin',(0.,-2.,7.55));
#4639=CARTESIAN_POINT('',(1.4,-2.,5.));
#4640=CARTESIAN_POINT('',(-1.4,-2.,5.));
#4641=CARTESIAN_POINT('',(1.4,-2.,10.));
#4642=CARTESIAN_POINT('',(1.4,-2.,5.));
#4643=CARTESIAN_POINT('',(-1.4,-2.,10.));
#4644=CARTESIAN_POINT('',(0.,-2.,10.));
#4645=CARTESIAN_POINT('',(-1.4,-2.,5.));
#4646=CARTESIAN_POINT('',(-1.4,-2.,10.1));
#4647=CARTESIAN_POINT('',(-1.4,-2.,5.));
#4648=CARTESIAN_POINT('Origin',(1.4,-2.,5.));
#4649=CARTESIAN_POINT('',(1.4,-1.5,5.));
#4650=CARTESIAN_POINT('',(-1.4,-1.5,5.));
#4651=CARTESIAN_POINT('',(1.4,-2.,5.));
#4652=CARTESIAN_POINT('Origin',(0.,2.,7.55));
#4653=CARTESIAN_POINT('',(-1.4,2.,5.));
#4654=CARTESIAN_POINT('',(-1.4,2.,5.));
#4655=CARTESIAN_POINT('',(-1.4,2.,10.));
#4656=CARTESIAN_POINT('',(-1.4,2.,10.1));
#4657=CARTESIAN_POINT('',(1.4,2.,10.));
#4658=CARTESIAN_POINT('',(0.,2.,10.));
#4659=CARTESIAN_POINT('',(1.4,2.,5.));
#4660=CARTESIAN_POINT('Origin',(1.4,1.5,10.1));
#4661=CARTESIAN_POINT('',(1.4,0.75,10.));
#4662=CARTESIAN_POINT('Origin',(-1.4,1.5,5.));
#4663=CARTESIAN_POINT('',(-1.4,0.75,10.));
#4664=CARTESIAN_POINT('',(-1.4,1.5,5.));
#4665=CARTESIAN_POINT('Origin',(1.4,1.5,5.));
#4666=CARTESIAN_POINT('Origin',(0.,-1.5,7.55));
#4667=CARTESIAN_POINT('',(-1.4,-1.5,5.));
#4668=CARTESIAN_POINT('',(-1.4,-1.5,5.));
#4669=CARTESIAN_POINT('',(-1.4,-1.5,10.));
#4670=CARTESIAN_POINT('',(-1.4,-1.5,10.1));
#4671=CARTESIAN_POINT('',(1.4,-1.5,10.));
#4672=CARTESIAN_POINT('',(0.,-1.5,10.));
#4673=CARTESIAN_POINT('',(1.4,-1.5,5.));
#4674=CARTESIAN_POINT('Origin',(1.4,-2.,10.1));
#4675=CARTESIAN_POINT('',(1.4,-1.,10.));
#4676=CARTESIAN_POINT('Origin',(-1.4,-2.,5.));
#4677=CARTESIAN_POINT('',(-1.4,-1.,10.));
#4678=CARTESIAN_POINT('',(-1.4,-2.,5.));
#4679=CARTESIAN_POINT('Origin',(1.4,-2.,5.));
#4680=CARTESIAN_POINT('Origin',(4.,-3.,9.9));
#4681=CARTESIAN_POINT('',(3.575,-3.,10.));
#4682=CARTESIAN_POINT('Origin',(4.,-3.,10.));
#4683=CARTESIAN_POINT('',(3.575,-3.,10.8));
#4684=CARTESIAN_POINT('',(3.575,-3.,9.9));
#4685=CARTESIAN_POINT('Origin',(4.,-3.,10.8));
#4686=CARTESIAN_POINT('Origin',(-4.,3.,9.9));
#4687=CARTESIAN_POINT('',(-4.425,3.,10.));
#4688=CARTESIAN_POINT('Origin',(-4.,3.,10.));
#4689=CARTESIAN_POINT('',(-4.425,3.,10.8));
#4690=CARTESIAN_POINT('',(-4.425,3.,9.9));
#4691=CARTESIAN_POINT('Origin',(-4.,3.,10.8));
#4692=CARTESIAN_POINT('Origin',(-4.,-3.,9.9));
#4693=CARTESIAN_POINT('',(-4.425,-3.,10.));
#4694=CARTESIAN_POINT('Origin',(-4.,-3.,10.));
#4695=CARTESIAN_POINT('',(-4.425,-3.,10.8));
#4696=CARTESIAN_POINT('',(-4.425,-3.,9.9));
#4697=CARTESIAN_POINT('Origin',(-4.,-3.,10.8));
#4698=CARTESIAN_POINT('Origin',(4.,3.,9.9));
#4699=CARTESIAN_POINT('',(3.575,3.,10.));
#4700=CARTESIAN_POINT('Origin',(4.,3.,10.));
#4701=CARTESIAN_POINT('',(3.575,3.,10.8));
#4702=CARTESIAN_POINT('',(3.575,3.,9.9));
#4703=CARTESIAN_POINT('Origin',(4.,3.,10.8));
#4704=CARTESIAN_POINT('Origin',(5.,4.,10.));
#4705=CARTESIAN_POINT('',(5.,4.,10.));
#4706=CARTESIAN_POINT('',(-5.,4.,10.));
#4707=CARTESIAN_POINT('',(5.,4.,10.));
#4708=CARTESIAN_POINT('',(-5.,4.,10.8));
#4709=CARTESIAN_POINT('',(-5.,4.,10.));
#4710=CARTESIAN_POINT('',(5.,4.,10.8));
#4711=CARTESIAN_POINT('',(5.,4.,10.8));
#4712=CARTESIAN_POINT('',(5.,4.,10.));
#4713=CARTESIAN_POINT('Origin',(5.,-4.,10.));
#4714=CARTESIAN_POINT('',(5.,-4.,10.));
#4715=CARTESIAN_POINT('',(5.,-4.,10.));
#4716=CARTESIAN_POINT('',(5.,-4.,10.8));
#4717=CARTESIAN_POINT('',(5.,-4.,10.8));
#4718=CARTESIAN_POINT('',(5.,-4.,10.));
#4719=CARTESIAN_POINT('Origin',(-5.,-4.,10.));
#4720=CARTESIAN_POINT('',(-5.,-4.,10.));
#4721=CARTESIAN_POINT('',(-5.,-4.,10.));
#4722=CARTESIAN_POINT('',(-5.,-4.,10.8));
#4723=CARTESIAN_POINT('',(-5.,-4.,10.8));
#4724=CARTESIAN_POINT('',(-5.,-4.,10.));
#4725=CARTESIAN_POINT('Origin',(-5.,4.,10.));
#4726=CARTESIAN_POINT('',(-5.,4.,10.));
#4727=CARTESIAN_POINT('',(-5.,4.,10.8));
#4728=CARTESIAN_POINT('Origin',(0.,0.,10.8));
#4729=CARTESIAN_POINT('Origin',(0.,0.,10.));
#4730=CARTESIAN_POINT('',(0.,0.,0.));
#4731=CARTESIAN_POINT('Origin',(0.,0.9,3.5));
#4732=CARTESIAN_POINT('',(-0.165,0.9,3.5));
#4733=CARTESIAN_POINT('Origin',(0.,0.9,3.5));
#4734=CARTESIAN_POINT('',(-0.165,2.,3.5));
#4735=CARTESIAN_POINT('',(-0.165,0.9,3.5));
#4736=CARTESIAN_POINT('Origin',(0.,2.,3.5));
#4737=CARTESIAN_POINT('Origin',(0.,0.9,3.5));
#4738=CARTESIAN_POINT('Origin',(0.,-2.,3.5));
#4739=CARTESIAN_POINT('',(-0.9,-2.,3.5));
#4740=CARTESIAN_POINT('Origin',(0.,-2.,3.5));
#4741=CARTESIAN_POINT('',(-0.6,-2.,3.5));
#4742=CARTESIAN_POINT('Origin',(0.,-2.,3.5));
#4743=CARTESIAN_POINT('Origin',(0.,-2.4,3.5));
#4744=CARTESIAN_POINT('',(-0.9,-2.4,3.5));
#4745=CARTESIAN_POINT('',(-0.9,-2.4,3.5));
#4746=CARTESIAN_POINT('Origin',(0.,-2.4,3.5));
#4747=CARTESIAN_POINT('Origin',(0.,-2.4,3.5));
#4748=CARTESIAN_POINT('Origin',(0.,-2.,3.5));
#4749=CARTESIAN_POINT('',(-0.6,2.,3.5));
#4750=CARTESIAN_POINT('Origin',(0.,2.,3.5));
#4751=CARTESIAN_POINT('',(-0.6,-2.,3.5));
#4752=CARTESIAN_POINT('Origin',(0.,2.,3.5));
#4753=CARTESIAN_POINT('',(0.,0.,0.));
#4754=CARTESIAN_POINT('Origin',(0.,4.5,10.));
#4755=CARTESIAN_POINT('',(-0.605,4.9,10.));
#4756=CARTESIAN_POINT('Origin',(0.,4.9,10.));
#4757=CARTESIAN_POINT('',(-0.605,4.5,10.));
#4758=CARTESIAN_POINT('',(-0.605,4.5,10.));
#4759=CARTESIAN_POINT('Origin',(0.,4.5,10.));
#4760=CARTESIAN_POINT('Origin',(0.,4.5,10.));
#4761=CARTESIAN_POINT('',(-0.8,4.9,10.));
#4762=CARTESIAN_POINT('Origin',(0.,4.9,10.));
#4763=CARTESIAN_POINT('',(-0.8,4.5,10.));
#4764=CARTESIAN_POINT('',(-0.8,4.5,10.));
#4765=CARTESIAN_POINT('Origin',(0.,4.5,10.));
#4766=CARTESIAN_POINT('Origin',(0.,4.9,10.));
#4767=CARTESIAN_POINT('Origin',(0.,4.5,10.));
#4768=CARTESIAN_POINT('',(0.,0.,0.));
#4769=CARTESIAN_POINT('Origin',(0.,2.2,4.));
#4770=CARTESIAN_POINT('',(-0.225,2.4,4.));
#4771=CARTESIAN_POINT('Origin',(0.,2.4,4.));
#4772=CARTESIAN_POINT('',(-0.225,2.2,4.));
#4773=CARTESIAN_POINT('',(-0.225,2.2,4.));
#4774=CARTESIAN_POINT('Origin',(0.,2.2,4.));
#4775=CARTESIAN_POINT('Origin',(0.,2.2,4.));
#4776=CARTESIAN_POINT('',(-0.8,2.4,4.));
#4777=CARTESIAN_POINT('Origin',(0.,2.4,4.));
#4778=CARTESIAN_POINT('',(-0.8,2.2,4.));
#4779=CARTESIAN_POINT('',(-0.8,2.2,4.));
#4780=CARTESIAN_POINT('Origin',(0.,2.2,4.));
#4781=CARTESIAN_POINT('Origin',(0.,2.4,4.));
#4782=CARTESIAN_POINT('Origin',(0.,2.2,4.));
#4783=CARTESIAN_POINT('',(0.,0.,0.));
#4784=CARTESIAN_POINT('Origin',(0.0866025403784439,-0.4,-0.15));
#4785=CARTESIAN_POINT('',(0.173205080756888,-0.4,0.));
#4786=CARTESIAN_POINT('',(0.0866025403784439,-0.4,-0.15));
#4787=CARTESIAN_POINT('',(0.173205080756888,-0.4,0.));
#4788=CARTESIAN_POINT('',(0.0866025403784439,-0.64,-0.15));
#4789=CARTESIAN_POINT('',(0.0866025403784439,-0.4,-0.15));
#4790=CARTESIAN_POINT('',(0.173205080756888,-0.64,0.));
#4791=CARTESIAN_POINT('',(0.173205080756888,-0.64,0.));
#4792=CARTESIAN_POINT('',(0.173205080756888,-0.4,0.));
#4793=CARTESIAN_POINT('Origin',(-0.0866025403784438,-0.4,-0.15));
#4794=CARTESIAN_POINT('',(-0.0866025403784438,-0.4,-0.15));
#4795=CARTESIAN_POINT('',(0.0866025403784439,-0.4,-0.15));
#4796=CARTESIAN_POINT('',(-0.0866025403784438,-0.64,-0.15));
#4797=CARTESIAN_POINT('',(-0.0866025403784438,-0.4,-0.15));
#4798=CARTESIAN_POINT('',(0.0866025403784439,-0.64,-0.15));
#4799=CARTESIAN_POINT('Origin',(-0.173205080756888,-0.4,-2.77555756156289E-17));
#4800=CARTESIAN_POINT('',(-0.173205080756888,-0.4,-2.12115047744981E-17));
#4801=CARTESIAN_POINT('',(-0.0866025403784438,-0.4,-0.15));
#4802=CARTESIAN_POINT('',(-0.173205080756888,-0.64,-2.77555756156289E-17));
#4803=CARTESIAN_POINT('',(-0.173205080756888,-0.4,-2.12115047744981E-17));
#4804=CARTESIAN_POINT('',(-0.0866025403784438,-0.64,-0.15));
#4805=CARTESIAN_POINT('Origin',(-0.0866025403784439,-0.4,0.15));
#4806=CARTESIAN_POINT('',(-0.0866025403784439,-0.4,0.15));
#4807=CARTESIAN_POINT('',(-0.173205080756888,-0.4,-2.12115047744981E-17));
#4808=CARTESIAN_POINT('',(-0.0866025403784439,-0.64,0.15));
#4809=CARTESIAN_POINT('',(-0.0866025403784439,-0.4,0.15));
#4810=CARTESIAN_POINT('',(-0.173205080756888,-0.64,-2.12115047744981E-17));
#4811=CARTESIAN_POINT('Origin',(0.0866025403784439,-0.4,0.15));
#4812=CARTESIAN_POINT('',(0.0866025403784439,-0.4,0.15));
#4813=CARTESIAN_POINT('',(-0.0866025403784439,-0.4,0.15));
#4814=CARTESIAN_POINT('',(0.0866025403784439,-0.64,0.15));
#4815=CARTESIAN_POINT('',(0.0866025403784439,-0.4,0.15));
#4816=CARTESIAN_POINT('',(-0.0866025403784439,-0.64,0.15));
#4817=CARTESIAN_POINT('Origin',(0.173205080756888,-0.4,0.));
#4818=CARTESIAN_POINT('',(0.0866025403784439,-0.4,0.15));
#4819=CARTESIAN_POINT('',(0.0866025403784439,-0.64,0.15));
#4820=CARTESIAN_POINT('Origin',(0.,-0.4,-2.77555756156289E-17));
#4821=CARTESIAN_POINT('Origin',(0.,-0.64,-2.77555756156289E-17));
#4822=CARTESIAN_POINT('Origin',(0.,-1.,0.));
#4823=CARTESIAN_POINT('',(-0.1954,-1.,2.39295984553393E-17));
#4824=CARTESIAN_POINT('Origin',(0.,-1.,0.));
#4825=CARTESIAN_POINT('Origin',(0.3,0.4,0.));
#4826=CARTESIAN_POINT('',(-0.3,0.4,-3.67394039744206E-17));
#4827=CARTESIAN_POINT('Origin',(0.,0.4,0.));
#4828=CARTESIAN_POINT('Origin',(0.,0.375,0.));
#4829=CARTESIAN_POINT('',(-0.35,0.35,-4.28626379701573E-17));
#4830=CARTESIAN_POINT('Origin',(0.,0.35,0.));
#4831=CARTESIAN_POINT('',(-0.325,0.375,-3.9801020972289E-17));
#4832=CARTESIAN_POINT('Origin',(0.,0.19,0.));
#4833=CARTESIAN_POINT('',(-0.35,0.03,-4.28626379701574E-17));
#4834=CARTESIAN_POINT('Origin',(0.,0.03,0.));
#4835=CARTESIAN_POINT('',(-0.35,0.19,-4.28626379701574E-17));
#4836=CARTESIAN_POINT('Origin',(0.,0.0149999999999999,0.));
#4837=CARTESIAN_POINT('',(-0.32,-3.29597460435593E-17,-3.91886975727153E-17));
#4838=CARTESIAN_POINT('Origin',(0.,0.,0.));
#4839=CARTESIAN_POINT('',(-0.335,0.0149999999999999,-4.10256677714363E-17));
#4840=CARTESIAN_POINT('Origin',(0.22,0.,0.));
#4841=CARTESIAN_POINT('',(-0.22,-6.93889390390723E-18,-2.69422295812418E-17));
#4842=CARTESIAN_POINT('Origin',(0.,0.,0.));
#4843=CARTESIAN_POINT('Origin',(0.,-0.02,0.));
#4844=CARTESIAN_POINT('',(-0.1954,-0.0492,2.39295984553393E-17));
#4845=CARTESIAN_POINT('Origin',(0.,-0.0492,0.));
#4846=CARTESIAN_POINT('',(-0.21,-0.02,-2.57175827820944E-17));
#4847=CARTESIAN_POINT('Origin',(0.,-0.8,0.));
#4848=CARTESIAN_POINT('',(-0.1954,-0.8,-2.39295984553393E-17));
#4849=CARTESIAN_POINT('',(0.,0.,0.));
#4850=CARTESIAN_POINT('Origin',(0.,0.,0.));
#4851=CARTESIAN_POINT('',(-0.32,0.16,3.91886975727153E-17));
#4852=CARTESIAN_POINT('Origin',(0.,0.16,0.));
#4853=CARTESIAN_POINT('',(-0.32,0.,3.91886975727153E-17));
#4854=CARTESIAN_POINT('',(-0.32,0.,3.91886975727153E-17));
#4855=CARTESIAN_POINT('Origin',(0.,0.,0.));
#4856=CARTESIAN_POINT('Origin',(0.,0.,0.));
#4857=CARTESIAN_POINT('',(-0.6,0.16,7.34788079488412E-17));
#4858=CARTESIAN_POINT('Origin',(0.,0.16,0.));
#4859=CARTESIAN_POINT('',(-0.6,0.,7.34788079488412E-17));
#4860=CARTESIAN_POINT('',(-0.6,0.,7.34788079488412E-17));
#4861=CARTESIAN_POINT('Origin',(0.,0.,0.));
#4862=CARTESIAN_POINT('Origin',(0.,0.16,0.));
#4863=CARTESIAN_POINT('Origin',(0.,0.,0.));
#4864=CARTESIAN_POINT('',(0.,0.,0.));
#4865=CARTESIAN_POINT('Origin',(0.,-1.445,0.));
#4866=CARTESIAN_POINT('',(-0.2942,-2.9458,3.60291088309151E-17));
#4867=CARTESIAN_POINT('Origin',(0.,-2.9458,0.));
#4868=CARTESIAN_POINT('',(-0.2942,0.,-3.60291088309151E-17));
#4869=CARTESIAN_POINT('',(-0.2942,-1.445,-3.60291088309151E-17));
#4870=CARTESIAN_POINT('Origin',(0.,0.,0.));
#4871=CARTESIAN_POINT('Origin',(0.,-2.97,0.));
#4872=CARTESIAN_POINT('',(-0.24,-3.,-2.93915231795365E-17));
#4873=CARTESIAN_POINT('Origin',(0.,-3.,0.));
#4874=CARTESIAN_POINT('',(-0.27,-2.97,-3.30654635769785E-17));
#4875=CARTESIAN_POINT('Origin',(0.,-3.,0.));
#4876=CARTESIAN_POINT('Origin',(0.,0.341586508806388,0.));
#4877=CARTESIAN_POINT('',(-0.475,0.4,-5.81707229594993E-17));
#4878=CARTESIAN_POINT('Origin',(0.,0.4,0.));
#4879=CARTESIAN_POINT('',(-0.577350269189626,0.340908044531739,-7.07050159149938E-17));
#4880=CARTESIAN_POINT('',(-0.576175134594813,0.341586508806388,-7.05611034329833E-17));
#4881=CARTESIAN_POINT('',(-0.288675134594813,0.340908044531739,0.5));
#4882=CARTESIAN_POINT('Ctrl Pts',(-0.288675134594813,0.340908044531739,
0.5));
#4883=CARTESIAN_POINT('Ctrl Pts',(-0.433012701893303,0.424241377863696,
0.249999999998124));
#4884=CARTESIAN_POINT('Ctrl Pts',(-0.577350269189626,0.340908044531739,
-7.07050159149938E-17));
#4885=CARTESIAN_POINT('',(0.288675134594813,0.340908044531739,0.5));
#4886=CARTESIAN_POINT('Ctrl Pts',(0.288675134594813,0.340908044531739,0.5));
#4887=CARTESIAN_POINT('Ctrl Pts',(-2.16648921025353E-12,0.424241377863696,
0.5));
#4888=CARTESIAN_POINT('Ctrl Pts',(-0.288675134594813,0.340908044531739,
0.5));
#4889=CARTESIAN_POINT('',(0.577350269189626,0.340908044531739,0.));
#4890=CARTESIAN_POINT('Ctrl Pts',(0.577350269189626,0.340908044531739,0.));
#4891=CARTESIAN_POINT('Ctrl Pts',(0.433012701891136,0.424241377863697,0.250000000001876));
#4892=CARTESIAN_POINT('Ctrl Pts',(0.288675134594813,0.340908044531739,0.5));
#4893=CARTESIAN_POINT('',(0.288675134594813,0.340908044531739,-0.5));
#4894=CARTESIAN_POINT('Ctrl Pts',(0.288675134594813,0.340908044531739,-0.5));
#4895=CARTESIAN_POINT('Ctrl Pts',(0.433012701893303,0.424241377863696,-0.249999999998124));
#4896=CARTESIAN_POINT('Ctrl Pts',(0.577350269189626,0.340908044531739,0.));
#4897=CARTESIAN_POINT('',(-0.288675134594813,0.340908044531739,-0.5));
#4898=CARTESIAN_POINT('Ctrl Pts',(-0.288675134594813,0.340908044531739,
-0.5));
#4899=CARTESIAN_POINT('Ctrl Pts',(2.16660023255599E-12,0.424241377863696,
-0.5));
#4900=CARTESIAN_POINT('Ctrl Pts',(0.288675134594813,0.340908044531739,-0.5));
#4901=CARTESIAN_POINT('Ctrl Pts',(-0.577350269189626,0.340908044531739,
-7.07050159149938E-17));
#4902=CARTESIAN_POINT('Ctrl Pts',(-0.433012701891136,0.424241377863697,
-0.250000000001876));
#4903=CARTESIAN_POINT('Ctrl Pts',(-0.288675134594813,0.340908044531739,
-0.5));
#4904=CARTESIAN_POINT('Origin',(0.288675134594813,0.,-0.5));
#4905=CARTESIAN_POINT('',(0.288675134594813,0.,-0.5));
#4906=CARTESIAN_POINT('',(0.288675134594813,0.,-0.5));
#4907=CARTESIAN_POINT('',(-0.288675134594813,0.,-0.5));
#4908=CARTESIAN_POINT('',(0.288675134594813,0.,-0.5));
#4909=CARTESIAN_POINT('',(-0.288675134594813,0.,-0.5));
#4910=CARTESIAN_POINT('Origin',(0.577350269189626,0.,0.));
#4911=CARTESIAN_POINT('',(0.577350269189626,0.,0.));
#4912=CARTESIAN_POINT('',(0.577350269189626,0.,0.));
#4913=CARTESIAN_POINT('',(0.577350269189626,0.,0.));
#4914=CARTESIAN_POINT('Origin',(0.288675134594813,0.,0.5));
#4915=CARTESIAN_POINT('',(0.288675134594813,0.,0.5));
#4916=CARTESIAN_POINT('',(0.288675134594813,0.,0.5));
#4917=CARTESIAN_POINT('',(0.288675134594813,0.,0.5));
#4918=CARTESIAN_POINT('Origin',(-0.288675134594813,0.,0.5));
#4919=CARTESIAN_POINT('',(-0.288675134594813,0.,0.5));
#4920=CARTESIAN_POINT('',(-0.288675134594813,0.,0.5));
#4921=CARTESIAN_POINT('',(-0.288675134594813,0.,0.5));
#4922=CARTESIAN_POINT('Origin',(-0.577350269189626,0.,-7.07050159149938E-17));
#4923=CARTESIAN_POINT('',(-0.577350269189626,0.,-7.07050159149938E-17));
#4924=CARTESIAN_POINT('',(-0.577350269189626,0.,-7.07050159149938E-17));
#4925=CARTESIAN_POINT('',(-0.577350269189626,0.,-7.07050159149938E-17));
#4926=CARTESIAN_POINT('Origin',(-0.288675134594813,0.,-0.5));
#4927=CARTESIAN_POINT('',(-0.288675134594813,0.,-0.5));
#4928=CARTESIAN_POINT('Origin',(0.,0.4,0.));
#4929=CARTESIAN_POINT('Origin',(0.,0.,0.));
#4930=CARTESIAN_POINT('',(0.,0.,0.));
#4931=CARTESIAN_POINT('Origin',(0.,0.0584134911936118,0.));
#4932=CARTESIAN_POINT('',(-0.288675134594813,0.0590919554682611,0.5));
#4933=CARTESIAN_POINT('',(0.288675134594813,0.0590919554682611,0.5));
#4934=CARTESIAN_POINT('Ctrl Pts',(-0.288675134594813,0.0590919554682611,
0.5));
#4935=CARTESIAN_POINT('Ctrl Pts',(2.1664336991023E-12,-0.0242413778636964,
0.5));
#4936=CARTESIAN_POINT('Ctrl Pts',(0.288675134594813,0.0590919554682611,
0.5));
#4937=CARTESIAN_POINT('',(-0.577350269189626,0.0590919554682611,-7.07050159149938E-17));
#4938=CARTESIAN_POINT('Ctrl Pts',(-0.577350269189626,0.0590919554682611,
-7.07050159149938E-17));
#4939=CARTESIAN_POINT('Ctrl Pts',(-0.433012701891136,-0.0242413778636963,
0.250000000001876));
#4940=CARTESIAN_POINT('Ctrl Pts',(-0.288675134594813,0.0590919554682611,
0.5));
#4941=CARTESIAN_POINT('',(-0.475,-4.16333634234434E-17,-5.81707229594993E-17));
#4942=CARTESIAN_POINT('',(-0.576175134594813,0.0584134911936118,-7.05611034329833E-17));
#4943=CARTESIAN_POINT('Origin',(0.,0.,0.));
#4944=CARTESIAN_POINT('',(-0.288675134594813,0.0590919554682611,-0.5));
#4945=CARTESIAN_POINT('Ctrl Pts',(-0.288675134594813,0.0590919554682611,
-0.5));
#4946=CARTESIAN_POINT('Ctrl Pts',(-0.433012701893303,-0.0242413778636963,
-0.249999999998124));
#4947=CARTESIAN_POINT('Ctrl Pts',(-0.577350269189626,0.0590919554682611,
-7.07050159149938E-17));
#4948=CARTESIAN_POINT('',(0.288675134594813,0.0590919554682611,-0.5));
#4949=CARTESIAN_POINT('Ctrl Pts',(0.288675134594813,0.0590919554682611,
-0.5));
#4950=CARTESIAN_POINT('Ctrl Pts',(-2.16648921025353E-12,-0.0242413778636962,
-0.5));
#4951=CARTESIAN_POINT('Ctrl Pts',(-0.288675134594813,0.0590919554682611,
-0.5));
#4952=CARTESIAN_POINT('',(0.577350269189626,0.0590919554682611,0.));
#4953=CARTESIAN_POINT('Ctrl Pts',(0.577350269189626,0.0590919554682611,
0.));
#4954=CARTESIAN_POINT('Ctrl Pts',(0.433012701891136,-0.0242413778636963,
-0.250000000001876));
#4955=CARTESIAN_POINT('Ctrl Pts',(0.288675134594813,0.0590919554682611,
-0.5));
#4956=CARTESIAN_POINT('Ctrl Pts',(0.288675134594813,0.0590919554682611,
0.5));
#4957=CARTESIAN_POINT('Ctrl Pts',(0.433012701893303,-0.0242413778636962,
0.249999999998124));
#4958=CARTESIAN_POINT('Ctrl Pts',(0.577350269189626,0.0590919554682611,
0.));
#4959=CARTESIAN_POINT('Origin',(0.,0.461586508806388,0.));
#4960=CARTESIAN_POINT('',(-0.475,0.52,-5.81707229594993E-17));
#4961=CARTESIAN_POINT('Origin',(0.,0.52,0.));
#4962=CARTESIAN_POINT('',(-0.577350269189626,0.460908044531739,-7.07050159149938E-17));
#4963=CARTESIAN_POINT('',(-0.576175134594813,0.461586508806388,-7.05611034329833E-17));
#4964=CARTESIAN_POINT('',(-0.288675134594813,0.460908044531739,0.5));
#4965=CARTESIAN_POINT('Ctrl Pts',(-0.288675134594813,0.460908044531739,
0.5));
#4966=CARTESIAN_POINT('Ctrl Pts',(-0.433012701893303,0.544241377863696,
0.249999999998124));
#4967=CARTESIAN_POINT('Ctrl Pts',(-0.577350269189626,0.460908044531739,
-7.07050159149938E-17));
#4968=CARTESIAN_POINT('',(0.288675134594813,0.460908044531739,0.5));
#4969=CARTESIAN_POINT('Ctrl Pts',(0.288675134594813,0.460908044531739,0.5));
#4970=CARTESIAN_POINT('Ctrl Pts',(-2.16676676600969E-12,0.544241377863697,
0.5));
#4971=CARTESIAN_POINT('Ctrl Pts',(-0.288675134594813,0.460908044531739,
0.5));
#4972=CARTESIAN_POINT('',(0.577350269189626,0.460908044531739,0.));
#4973=CARTESIAN_POINT('Ctrl Pts',(0.577350269189626,0.460908044531739,0.));
#4974=CARTESIAN_POINT('Ctrl Pts',(0.433012701891136,0.544241377863696,0.250000000001876));
#4975=CARTESIAN_POINT('Ctrl Pts',(0.288675134594813,0.460908044531739,0.5));
#4976=CARTESIAN_POINT('',(0.288675134594813,0.460908044531739,-0.5));
#4977=CARTESIAN_POINT('Ctrl Pts',(0.288675134594813,0.460908044531739,-0.5));
#4978=CARTESIAN_POINT('Ctrl Pts',(0.433012701893302,0.544241377863696,-0.249999999998124));
#4979=CARTESIAN_POINT('Ctrl Pts',(0.577350269189626,0.460908044531739,0.));
#4980=CARTESIAN_POINT('',(-0.288675134594813,0.460908044531739,-0.5));
#4981=CARTESIAN_POINT('Ctrl Pts',(-0.288675134594813,0.460908044531739,
-0.5));
#4982=CARTESIAN_POINT('Ctrl Pts',(2.16660023255599E-12,0.544241377863697,
-0.5));
#4983=CARTESIAN_POINT('Ctrl Pts',(0.288675134594813,0.460908044531739,-0.5));
#4984=CARTESIAN_POINT('Ctrl Pts',(-0.577350269189626,0.460908044531739,
-7.07050159149938E-17));
#4985=CARTESIAN_POINT('Ctrl Pts',(-0.433012701891136,0.544241377863696,
-0.250000000001876));
#4986=CARTESIAN_POINT('Ctrl Pts',(-0.288675134594813,0.460908044531739,
-0.5));
#4987=CARTESIAN_POINT('Origin',(0.288675134594813,0.,-0.5));
#4988=CARTESIAN_POINT('',(-0.288675134594813,0.,-0.5));
#4989=CARTESIAN_POINT('',(0.288675134594813,0.,-0.5));
#4990=CARTESIAN_POINT('Origin',(-0.288675134594813,0.,-0.5));
#4991=CARTESIAN_POINT('',(-0.577350269189626,0.,-7.07050159149938E-17));
#4992=CARTESIAN_POINT('Origin',(-0.577350269189626,0.,-7.07050159149938E-17));
#4993=CARTESIAN_POINT('',(-0.288675134594813,0.,0.5));
#4994=CARTESIAN_POINT('Origin',(0.,0.,0.));
#4995=CARTESIAN_POINT('',(-0.25175,0.52,3.08304831685346E-17));
#4996=CARTESIAN_POINT('Origin',(0.,0.52,0.));
#4997=CARTESIAN_POINT('',(-0.25175,0.,3.08304831685346E-17));
#4998=CARTESIAN_POINT('',(-0.25175,0.,3.08304831685346E-17));
#4999=CARTESIAN_POINT('Origin',(0.,0.,0.));
#5000=CARTESIAN_POINT('Origin',(-0.288675134594813,0.,0.5));
#5001=CARTESIAN_POINT('',(0.288675134594813,0.,0.5));
#5002=CARTESIAN_POINT('Origin',(0.577350269189626,0.,0.));
#5003=CARTESIAN_POINT('',(0.577350269189626,0.,0.));
#5004=CARTESIAN_POINT('Origin',(0.288675134594813,0.,0.5));
#5005=CARTESIAN_POINT('Origin',(0.,0.52,0.));
#5006=CARTESIAN_POINT('Origin',(0.,0.,0.));
#5007=CARTESIAN_POINT('',(0.,0.,0.));
#5008=CARTESIAN_POINT('',(0.,0.,1.5));
#5009=CARTESIAN_POINT('',(0.,-3.4,-5.));
#5010=CARTESIAN_POINT('',(0.,-6.,-5.));
#5011=CARTESIAN_POINT('',(0.,-0.2,1.));
#5012=CARTESIAN_POINT('',(0.,2.2,5.));
#5013=CARTESIAN_POINT('',(-3.,-1.18,9.));
#5014=CARTESIAN_POINT('',(-3.,1.02,9.));
#5015=CARTESIAN_POINT('',(-3.,1.18,9.));
#5016=CARTESIAN_POINT('',(-3.,-1.7,9.));
#5017=CARTESIAN_POINT('',(0.,0.,0.));
#5018=CARTESIAN_POINT('',(0.,0.,0.));
#5019=CARTESIAN_POINT('Origin',(0.,0.1,4.));
#5020=CARTESIAN_POINT('',(-1.6,0.1,4.));
#5021=CARTESIAN_POINT('Origin',(0.,0.1,4.));
#5022=CARTESIAN_POINT('',(-1.6,1.2,4.));
#5023=CARTESIAN_POINT('',(-1.6,0.1,4.));
#5024=CARTESIAN_POINT('Origin',(0.,1.2,4.));
#5025=CARTESIAN_POINT('Origin',(0.,0.1,4.));
#5026=CARTESIAN_POINT('',(-0.62,0.1,4.));
#5027=CARTESIAN_POINT('Origin',(0.,0.1,4.));
#5028=CARTESIAN_POINT('Origin',(0.,-1.3,4.));
#5029=CARTESIAN_POINT('',(-1.6,-1.2,4.));
#5030=CARTESIAN_POINT('Origin',(0.,-1.2,4.));
#5031=CARTESIAN_POINT('',(-1.6,-0.0999999999999999,4.));
#5032=CARTESIAN_POINT('',(-1.6,-1.3,4.));
#5033=CARTESIAN_POINT('Origin',(0.,-0.0999999999999999,4.));
#5034=CARTESIAN_POINT('Origin',(0.,-0.0999999999999999,4.));
#5035=CARTESIAN_POINT('',(-0.62,-0.0999999999999999,4.));
#5036=CARTESIAN_POINT('Origin',(0.,-0.0999999999999999,4.));
#5037=CARTESIAN_POINT('Origin',(0.,-1.3,4.));
#5038=CARTESIAN_POINT('',(-0.62,-1.3,4.));
#5039=CARTESIAN_POINT('Origin',(0.,-1.2,4.));
#5040=CARTESIAN_POINT('',(-3.75,1.2,4.));
#5041=CARTESIAN_POINT('Origin',(0.,1.2,4.));
#5042=CARTESIAN_POINT('',(-3.75,-1.2,4.));
#5043=CARTESIAN_POINT('',(-3.75,-1.2,4.));
#5044=CARTESIAN_POINT('Origin',(0.,-1.2,4.));
#5045=CARTESIAN_POINT('Origin',(0.,1.2,4.));
#5046=CARTESIAN_POINT('Origin',(0.,-1.2,4.));
#5047=CARTESIAN_POINT('',(0.,0.,0.));
#5048=CARTESIAN_POINT('',(0.,0.,0.));
#5049=CARTESIAN_POINT('Origin',(0.,0.,0.));
#5050=CARTESIAN_POINT('',(-1.070235,-0.308121667383195,-1.31065986708547E-16));
#5051=CARTESIAN_POINT('',(-1.31065986708547E-16,-0.308121667383195,1.070235));
#5052=CARTESIAN_POINT('Origin',(0.,-0.308121667383195,0.));
#5053=CARTESIAN_POINT('Origin',(0.,-0.308121667383195,0.));
#5054=CARTESIAN_POINT('',(-1.31065986708547E-16,0.308121667383195,1.070235));
#5055=CARTESIAN_POINT('Origin',(-1.34711147906209E-16,0.,1.1));
#5056=CARTESIAN_POINT('',(-1.070235,0.308121667383195,1.31065986708547E-16));
#5057=CARTESIAN_POINT('Origin',(0.,0.308121667383195,0.));
#5058=CARTESIAN_POINT('Origin',(0.,0.308121667383195,0.));
#5059=CARTESIAN_POINT('Origin',(0.,0.,0.));
#5060=CARTESIAN_POINT('',(-1.070235,0.5,-1.31065986708547E-16));
#5061=CARTESIAN_POINT('',(-1.070235,0.,-1.31065986708547E-16));
#5062=CARTESIAN_POINT('Origin',(0.,0.5,0.));
#5063=CARTESIAN_POINT('Origin',(0.,0.,0.));
#5064=CARTESIAN_POINT('',(-0.6,-0.44,-7.34788079488412E-17));
#5065=CARTESIAN_POINT('Origin',(0.,-0.44,0.));
#5066=CARTESIAN_POINT('',(-0.6,0.44,-7.34788079488412E-17));
#5067=CARTESIAN_POINT('',(-0.6,0.,-7.34788079488412E-17));
#5068=CARTESIAN_POINT('Origin',(0.,0.44,0.));
#5069=CARTESIAN_POINT('Origin',(0.,0.47,0.));
#5070=CARTESIAN_POINT('',(-0.66,0.5,-8.08266887437253E-17));
#5071=CARTESIAN_POINT('',(-0.63,0.47,-7.71527483462832E-17));
#5072=CARTESIAN_POINT('Origin',(0.,0.5,0.));
#5073=CARTESIAN_POINT('Origin',(1.070235,0.5,0.));
#5074=CARTESIAN_POINT('Origin',(0.,0.,0.));
#5075=CARTESIAN_POINT('',(-1.070235,-0.5,-1.31065986708547E-16));
#5076=CARTESIAN_POINT('Origin',(0.,-0.5,0.));
#5077=CARTESIAN_POINT('',(-1.070235,0.,-1.31065986708547E-16));
#5078=CARTESIAN_POINT('Origin',(0.66,-0.5,0.));
#5079=CARTESIAN_POINT('',(-0.66,-0.5,-8.08266887437253E-17));
#5080=CARTESIAN_POINT('Origin',(0.,-0.5,0.));
#5081=CARTESIAN_POINT('Origin',(0.,-0.47,0.));
#5082=CARTESIAN_POINT('',(-0.63,-0.47,-7.71527483462832E-17));
#5083=CARTESIAN_POINT('',(0.,0.,0.));
#5084=CARTESIAN_POINT('Origin',(0.,0.,0.));
#5085=CARTESIAN_POINT('',(-1.129765,0.308121667383195,-1.38356309103871E-16));
#5086=CARTESIAN_POINT('',(-1.38356309103871E-16,0.308121667383195,1.129765));
#5087=CARTESIAN_POINT('Origin',(0.,0.308121667383195,0.));
#5088=CARTESIAN_POINT('Origin',(0.,0.308121667383195,0.));
#5089=CARTESIAN_POINT('',(-1.38356309103871E-16,-0.308121667383195,1.129765));
#5090=CARTESIAN_POINT('Origin',(-1.34711147906209E-16,0.,1.1));
#5091=CARTESIAN_POINT('',(-1.129765,-0.308121667383195,1.38356309103871E-16));
#5092=CARTESIAN_POINT('Origin',(0.,-0.308121667383195,0.));
#5093=CARTESIAN_POINT('Origin',(0.,-0.308121667383195,0.));
#5094=CARTESIAN_POINT('Origin',(0.,0.,0.));
#5095=CARTESIAN_POINT('',(-1.129765,-0.5,-1.38356309103871E-16));
#5096=CARTESIAN_POINT('Origin',(0.,-0.5,0.));
#5097=CARTESIAN_POINT('',(-1.129765,0.,-1.38356309103871E-16));
#5098=CARTESIAN_POINT('Origin',(1.54,0.5,0.));
#5099=CARTESIAN_POINT('',(-1.54,0.5,-1.88595607068692E-16));
#5100=CARTESIAN_POINT('Origin',(0.,0.5,0.));
#5101=CARTESIAN_POINT('',(-1.129765,0.5,-1.38356309103871E-16));
#5102=CARTESIAN_POINT('Origin',(0.,0.5,0.));
#5103=CARTESIAN_POINT('Origin',(0.,0.47,0.));
#5104=CARTESIAN_POINT('',(-1.6,0.44,-1.95943487863577E-16));
#5105=CARTESIAN_POINT('Origin',(0.,0.44,0.));
#5106=CARTESIAN_POINT('',(-1.57,0.47,-1.92269547466134E-16));
#5107=CARTESIAN_POINT('Origin',(0.,0.,0.));
#5108=CARTESIAN_POINT('',(-1.6,-0.44,-1.95943487863577E-16));
#5109=CARTESIAN_POINT('Origin',(0.,-0.44,0.));
#5110=CARTESIAN_POINT('',(-1.6,0.,-1.95943487863577E-16));
#5111=CARTESIAN_POINT('Origin',(0.,-0.47,0.));
#5112=CARTESIAN_POINT('',(-1.54,-0.5,-1.88595607068692E-16));
#5113=CARTESIAN_POINT('Origin',(0.,-0.5,0.));
#5114=CARTESIAN_POINT('',(-1.57,-0.47,-1.92269547466134E-16));
#5115=CARTESIAN_POINT('Origin',(1.129765,-0.5,0.));
#5116=CARTESIAN_POINT('Origin',(0.,0.,0.));
#5117=CARTESIAN_POINT('',(-1.129765,0.,-1.38356309103871E-16));
#5118=CARTESIAN_POINT('',(0.,0.,0.));
#5119=CARTESIAN_POINT('Origin',(1.1,0.,0.));
#5120=CARTESIAN_POINT('',(1.1,-2.23201749654651E-33,0.29765));
#5121=CARTESIAN_POINT('',(1.1,-2.23201749654651E-33,-0.29765));
#5122=CARTESIAN_POINT('Origin',(1.1,0.,0.));
#5123=CARTESIAN_POINT('Origin',(0.685838782044607,0.,-0.860014630714833));
#5124=CARTESIAN_POINT('',(0.918550922801216,-5.31350540756609E-33,-0.674432891191581));
#5125=CARTESIAN_POINT('',(0.453126641287998,8.49470414473068E-34,-1.04559637023808));
#5126=CARTESIAN_POINT('Origin',(0.685838782044607,0.,-0.860014630714833));
#5127=CARTESIAN_POINT('Origin',(-0.244773027351946,0.,-1.07242070340001));
#5128=CARTESIAN_POINT('',(0.0454142657089739,-2.23201749654651E-33,-1.1386540593921));
#5129=CARTESIAN_POINT('',(-0.534960320412865,-2.23201749654651E-33,-1.00618734740791));
#5130=CARTESIAN_POINT('Origin',(-0.244773027351946,0.,-1.07242070340001));
#5131=CARTESIAN_POINT('Origin',(-0.991065754692661,0.,-0.477272113029314));
#5132=CARTESIAN_POINT('',(-0.86192025974432,8.49470414473067E-34,-0.745445496560469));
#5133=CARTESIAN_POINT('',(-1.120211249641,-5.31350540756609E-33,-0.209098729498159));
#5134=CARTESIAN_POINT('Origin',(-0.991065754692661,0.,-0.477272113029314));
#5135=CARTESIAN_POINT('Origin',(-0.991065754692661,0.,0.477272113029314));
#5136=CARTESIAN_POINT('',(-1.120211249641,-2.23201749654651E-33,0.209098729498159));
#5137=CARTESIAN_POINT('',(-0.86192025974432,-2.23201749654651E-33,0.745445496560469));
#5138=CARTESIAN_POINT('Origin',(-0.991065754692661,0.,0.477272113029314));
#5139=CARTESIAN_POINT('Origin',(-0.244773027351946,0.,1.07242070340001));
#5140=CARTESIAN_POINT('',(-0.534960320412866,-2.23201749654651E-33,1.00618734740791));
#5141=CARTESIAN_POINT('',(0.0454142657089737,-2.23201749654651E-33,1.1386540593921));
#5142=CARTESIAN_POINT('Origin',(-0.244773027351946,0.,1.07242070340001));
#5143=CARTESIAN_POINT('Origin',(0.685838782044607,0.,0.860014630714833));
#5144=CARTESIAN_POINT('',(0.453126641287998,-2.23201749654651E-33,1.04559637023808));
#5145=CARTESIAN_POINT('',(0.918550922801216,-2.23201749654651E-33,0.674432891191581));
#5146=CARTESIAN_POINT('Origin',(0.685838782044607,0.,0.860014630714833));
#5147=CARTESIAN_POINT('',(0.,0.,0.));
#5148=CARTESIAN_POINT('Origin',(0.685838782044607,0.,0.860014630714833));
#5149=CARTESIAN_POINT('',(0.413083465285518,-0.05953,0.993751811093549));
#5150=CARTESIAN_POINT('',(0.876916659919095,-0.05953,0.623857181492959));
#5151=CARTESIAN_POINT('Ctrl Pts',(0.413083465285518,-0.05953,0.993751811093549));
#5152=CARTESIAN_POINT('Ctrl Pts',(0.419070565453383,-0.0925528133349865,
0.991263089003441));
#5153=CARTESIAN_POINT('Ctrl Pts',(0.430199341854858,-0.124911173756694,
0.986608710139579));
#5154=CARTESIAN_POINT('Ctrl Pts',(0.457978755888596,-0.177924977804098,
0.973971221090534));
#5155=CARTESIAN_POINT('Ctrl Pts',(0.473077587363685,-0.199697230012983,
0.966820759530997));
#5156=CARTESIAN_POINT('Ctrl Pts',(0.507057380724533,-0.237895043532788,
0.949440676105255));
#5157=CARTESIAN_POINT('Ctrl Pts',(0.525933334162555,-0.254319232363049,
0.939198248544428));
#5158=CARTESIAN_POINT('Ctrl Pts',(0.564362943424238,-0.28018331644634,0.916597376014514));
#5159=CARTESIAN_POINT('Ctrl Pts',(0.585840553788742,-0.29104845371857,0.903141581680914));
#5160=CARTESIAN_POINT('Ctrl Pts',(0.629305439856167,-0.30527573347708,0.873412008702649));
#5161=CARTESIAN_POINT('Ctrl Pts',(0.651278921914856,-0.308638795020976,
0.857118508332695));
#5162=CARTESIAN_POINT('Ctrl Pts',(0.690705563850638,-0.308638795020976,
0.825676810575914));
#5163=CARTESIAN_POINT('Ctrl Pts',(0.711480111898423,-0.30527573347708,0.807879894508811));
#5164=CARTESIAN_POINT('Ctrl Pts',(0.750136149454208,-0.29104845371857,0.772120216227122));
#5165=CARTESIAN_POINT('Ctrl Pts',(0.768033796848072,-0.28018331644634,0.754175290318038));
#5166=CARTESIAN_POINT('Ctrl Pts',(0.798619410861634,-0.254319232363049,
0.721738358858166));
#5167=CARTESIAN_POINT('Ctrl Pts',(0.812805334167529,-0.237895043532788,
0.705614819529209));
#5168=CARTESIAN_POINT('Ctrl Pts',(0.837310877969633,-0.199697230012983,
0.676354402927683));
#5169=CARTESIAN_POINT('Ctrl Pts',(0.847641868610495,-0.177924977804098,
0.663225258065736));
#5170=CARTESIAN_POINT('Ctrl Pts',(0.866144010579847,-0.124911173756694,
0.638954437806245));
#5171=CARTESIAN_POINT('Ctrl Pts',(0.873158080166742,-0.0925528133349865,
0.62914037979579));
#5172=CARTESIAN_POINT('Ctrl Pts',(0.876916659919095,-0.05953,0.623857181492959));
#5173=CARTESIAN_POINT('',(0.437601487681057,-0.05953,1.03511272300331));
#5174=CARTESIAN_POINT('Origin',(0.685838782044607,-0.05953,0.860014630714833));
#5175=CARTESIAN_POINT('',(0.911784794170997,-0.05953,0.656964154625313));
#5176=CARTESIAN_POINT('Ctrl Pts',(0.911784794170998,-0.0595300000000001,
0.656964154625312));
#5177=CARTESIAN_POINT('Ctrl Pts',(0.909827729890942,-0.0762225747374255,
0.659680317203144));
#5178=CARTESIAN_POINT('Ctrl Pts',(0.907004864562642,-0.0928409665394228,
0.663576540841106));
#5179=CARTESIAN_POINT('Ctrl Pts',(0.895234408667242,-0.144299303100741,
0.679480524217551));
#5180=CARTESIAN_POINT('Ctrl Pts',(0.882797231409153,-0.177024326825049,
0.695831250979106));
#5181=CARTESIAN_POINT('Ctrl Pts',(0.854332839576145,-0.227269801620064,
0.73042219438957));
#5182=CARTESIAN_POINT('Ctrl Pts',(0.834863020612702,-0.251265615809407,
0.752807465209441));
#5183=CARTESIAN_POINT('Ctrl Pts',(0.800439809856111,-0.279889827963178,
0.789147407129766));
#5184=CARTESIAN_POINT('Ctrl Pts',(0.781998747691871,-0.290879136862659,
0.80756613568454));
#5185=CARTESIAN_POINT('Ctrl Pts',(0.742239891936898,-0.305251990234487,
0.844254137480382));
#5186=CARTESIAN_POINT('Ctrl Pts',(0.720906778729541,-0.308638795020976,
0.862505527716294));
#5187=CARTESIAN_POINT('Ctrl Pts',(0.680463863683392,-0.308638795020976,
0.894757676234429));
#5188=CARTESIAN_POINT('Ctrl Pts',(0.657923009631182,-0.305251990234488,
0.91149460735272));
#5189=CARTESIAN_POINT('Ctrl Pts',(0.613307674922609,-0.290879136862659,
0.942092777160053));
#5190=CARTESIAN_POINT('Ctrl Pts',(0.591247219971725,-0.279889827963178,
0.955972930713954));
#5191=CARTESIAN_POINT('Ctrl Pts',(0.548158511259202,-0.251265615809407,
0.981446681891443));
#5192=CARTESIAN_POINT('Ctrl Pts',(0.522002043615455,-0.227269801620063,
0.995447160474328));
#5193=CARTESIAN_POINT('Ctrl Pts',(0.481944444320713,-0.177024326825049,
1.01550068154148));
#5194=CARTESIAN_POINT('Ctrl Pts',(0.463236132117164,-0.14429930310074,1.0239876538093));
#5195=CARTESIAN_POINT('Ctrl Pts',(0.445111721969657,-0.0928409665394226,
1.03192403056628));
#5196=CARTESIAN_POINT('Ctrl Pts',(0.440685038163619,-0.0762225747374254,
1.03380912944435));
#5197=CARTESIAN_POINT('Ctrl Pts',(0.437601487681056,-0.05953,1.03511272300331));
#5198=CARTESIAN_POINT('Origin',(0.685838782044607,-0.05953,0.860014630714833));
#5199=CARTESIAN_POINT('Origin',(0.,-0.208355,0.));
#5200=CARTESIAN_POINT('',(0.0548532617164168,-0.05953,1.12247250791415));
#5201=CARTESIAN_POINT('Origin',(0.,-0.05953,0.));
#5202=CARTESIAN_POINT('',(-0.536443649899848,-0.05953,0.987512846410683));
#5203=CARTESIAN_POINT('Ctrl Pts',(0.0548532617164173,-0.0595300000000001,
1.12247250791414));
#5204=CARTESIAN_POINT('Ctrl Pts',(0.05150947068137,-0.0762225747374254,
1.12263591311425));
#5205=CARTESIAN_POINT('Ctrl Pts',(0.0467032526342597,-0.0928409665394227,
1.12285816383385));
#5206=CARTESIAN_POINT('Ctrl Pts',(0.0269302585198975,-0.144299303100741,
1.12357162229597));
#5207=CARTESIAN_POINT('Ctrl Pts',(0.006392292392153,-0.177024326825049,
1.12404235695137));
#5208=CARTESIAN_POINT('Ctrl Pts',(-0.0383992541984087,-0.227269801620063,
1.12335509974011));
#5209=CARTESIAN_POINT('Ctrl Pts',(-0.0680399972366993,-0.251265615809407,
1.12208997038458));
#5210=CARTESIAN_POINT('Ctrl Pts',(-0.117914228755037,-0.279889827963178,
1.1178344036749));
#5211=CARTESIAN_POINT('Ctrl Pts',(-0.14381238480104,-0.290879136862659,
1.11490049012186));
#5212=CARTESIAN_POINT('Ctrl Pts',(-0.19728546073067,-0.305251990234488,
1.10669035995599));
#5213=CARTESIAN_POINT('Ctrl Pts',(-0.224855950742601,-0.308638795020976,
1.10139101611326));
#5214=CARTESIAN_POINT('Ctrl Pts',(-0.275287440920027,-0.308638795020976,
1.0898803575765));
#5215=CARTESIAN_POINT('Ctrl Pts',(-0.302426893214945,-0.305251990234488,
1.08269251410343));
#5216=CARTESIAN_POINT('Ctrl Pts',(-0.35416671187353,-0.290879136862659,
1.06688848765783));
#5217=CARTESIAN_POINT('Ctrl Pts',(-0.3787731215897,-0.279889827963178,1.05829506364875));
#5218=CARTESIAN_POINT('Ctrl Pts',(-0.425554672694338,-0.251265615809407,
1.04048957871266));
#5219=CARTESIAN_POINT('Ctrl Pts',(-0.452808978448581,-0.227269801620063,
1.02876878445619));
#5220=CARTESIAN_POINT('Ctrl Pts',(-0.493462957200432,-0.177024326825049,
1.0099536580922));
#5221=CARTESIAN_POINT('Ctrl Pts',(-0.511762781179148,-0.14429930310074,
1.00061845128527));
#5222=CARTESIAN_POINT('Ctrl Pts',(-0.529268075276157,-0.0928409665394226,
0.991396466802468));
#5223=CARTESIAN_POINT('Ctrl Pts',(-0.533501897135713,-0.0762225747374254,
0.989110885965947));
#5224=CARTESIAN_POINT('Ctrl Pts',(-0.536443649899848,-0.0595300000000001,
0.987512846410683));
#5225=CARTESIAN_POINT('',(-0.843383895613249,-0.05953,0.742736168477219));
#5226=CARTESIAN_POINT('Origin',(0.,-0.05953,0.));
#5227=CARTESIAN_POINT('',(-1.10653577764992,-0.05953,0.196295654879792));
#5228=CARTESIAN_POINT('Ctrl Pts',(-0.843383895613249,-0.0595300000000001,
0.742736168477219));
#5229=CARTESIAN_POINT('Ctrl Pts',(-0.84559647055299,-0.0762225747374255,
0.740223768851062));
#5230=CARTESIAN_POINT('Ctrl Pts',(-0.848766861100456,-0.0928409665394227,
0.736604687327351));
#5231=CARTESIAN_POINT('Ctrl Pts',(-0.861652925570091,-0.144299303100741,
0.721590372101268));
#5232=CARTESIAN_POINT('Ctrl Pts',(-0.87482617317514,-0.177024326825049,
0.705826641853758));
#5233=CARTESIAN_POINT('Ctrl Pts',(-0.902215926359523,-0.227269801620063,
0.670378702718353));
#5234=CARTESIAN_POINT('Ctrl Pts',(-0.919707509403859,-0.251265615809407,
0.646415841396062));
#5235=CARTESIAN_POINT('Ctrl Pts',(-0.947476448101718,-0.279889827963178,
0.604769294586516));
#5236=CARTESIAN_POINT('Ctrl Pts',(-0.961329858300736,-0.290879136862659,
0.582692035672022));
#5237=CARTESIAN_POINT('Ctrl Pts',(-0.988250837578047,-0.305251990234488,
0.535766169015486));
#5238=CARTESIAN_POINT('Ctrl Pts',(-1.00129756308006,-0.308638795020976,
0.510906605094603));
#5239=CARTESIAN_POINT('Ctrl Pts',(-1.02374168767024,-0.308638795020976,
0.46430090015576));
#5240=CARTESIAN_POINT('Ctrl Pts',(-1.03504317708586,-0.305251990234488,
0.438600874831839));
#5241=CARTESIAN_POINT('Ctrl Pts',(-1.05494634094458,-0.290879136862659,
0.388295406390235));
#5242=CARTESIAN_POINT('Ctrl Pts',(-1.06356957703048,-0.279889827963178,
0.363699428370917));
#5243=CARTESIAN_POINT('Ctrl Pts',(-1.0788165083757,-0.251265615809407,0.316022600643821));
#5244=CARTESIAN_POINT('Ctrl Pts',(-1.08664560412098,-0.227269801620063,
0.287406530683752));
#5245=CARTESIAN_POINT('Ctrl Pts',(-1.09728268713976,-0.177024326825049,
0.243890930799337));
#5246=CARTESIAN_POINT('Ctrl Pts',(-1.10139388218929,-0.144299303100741,
0.22376314604679));
#5247=CARTESIAN_POINT('Ctrl Pts',(-1.10509821673782,-0.0928409665394227,
0.204327142733961));
#5248=CARTESIAN_POINT('Ctrl Pts',(-1.10595102243643,-0.0762225747374254,
0.199591971170104));
#5249=CARTESIAN_POINT('Ctrl Pts',(-1.10653577764992,-0.0595300000000001,
0.196295654879792));
#5250=CARTESIAN_POINT('',(-1.123812,-0.05953,1.37627276864339E-16));
#5251=CARTESIAN_POINT('Origin',(0.,-0.05953,0.));
#5252=CARTESIAN_POINT('',(-1.123812,-0.35718,1.37627276864339E-16));
#5253=CARTESIAN_POINT('',(-1.123812,-0.208355,1.37627276864339E-16));
#5254=CARTESIAN_POINT('Origin',(0.,-0.35718,0.));
#5255=CARTESIAN_POINT('',(-1.10653577764992,-0.05953,-0.196295654879793));
#5256=CARTESIAN_POINT('Origin',(0.,-0.05953,0.));
#5257=CARTESIAN_POINT('',(-0.843383895613249,-0.05953,-0.742736168477219));
#5258=CARTESIAN_POINT('Ctrl Pts',(-1.10653577764992,-0.0595300000000001,
-0.196295654879792));
#5259=CARTESIAN_POINT('Ctrl Pts',(-1.10595102243643,-0.0762225747374255,
-0.199591971170104));
#5260=CARTESIAN_POINT('Ctrl Pts',(-1.10509821673782,-0.0928409665394228,
-0.204327142733962));
#5261=CARTESIAN_POINT('Ctrl Pts',(-1.10139388218929,-0.144299303100741,
-0.22376314604679));
#5262=CARTESIAN_POINT('Ctrl Pts',(-1.09728268713976,-0.177024326825049,
-0.243890930799338));
#5263=CARTESIAN_POINT('Ctrl Pts',(-1.08664560412098,-0.227269801620063,
-0.287406530683753));
#5264=CARTESIAN_POINT('Ctrl Pts',(-1.0788165083757,-0.251265615809407,-0.316022600643821));
#5265=CARTESIAN_POINT('Ctrl Pts',(-1.06356957703048,-0.279889827963178,
-0.363699428370918));
#5266=CARTESIAN_POINT('Ctrl Pts',(-1.05494634094458,-0.290879136862659,
-0.388295406390235));
#5267=CARTESIAN_POINT('Ctrl Pts',(-1.03504317708586,-0.305251990234488,
-0.438600874831839));
#5268=CARTESIAN_POINT('Ctrl Pts',(-1.02374168767024,-0.308638795020976,
-0.46430090015576));
#5269=CARTESIAN_POINT('Ctrl Pts',(-1.00129756308006,-0.308638795020976,
-0.510906605094603));
#5270=CARTESIAN_POINT('Ctrl Pts',(-0.988250837578047,-0.305251990234488,
-0.535766169015486));
#5271=CARTESIAN_POINT('Ctrl Pts',(-0.961329858300736,-0.290879136862659,
-0.582692035672022));
#5272=CARTESIAN_POINT('Ctrl Pts',(-0.947476448101718,-0.279889827963178,
-0.604769294586516));
#5273=CARTESIAN_POINT('Ctrl Pts',(-0.919707509403859,-0.251265615809407,
-0.646415841396062));
#5274=CARTESIAN_POINT('Ctrl Pts',(-0.902215926359523,-0.227269801620064,
-0.670378702718353));
#5275=CARTESIAN_POINT('Ctrl Pts',(-0.87482617317514,-0.177024326825049,
-0.705826641853758));
#5276=CARTESIAN_POINT('Ctrl Pts',(-0.861652925570091,-0.144299303100741,
-0.721590372101268));
#5277=CARTESIAN_POINT('Ctrl Pts',(-0.848766861100456,-0.0928409665394229,
-0.736604687327351));
#5278=CARTESIAN_POINT('Ctrl Pts',(-0.84559647055299,-0.0762225747374255,
-0.740223768851063));
#5279=CARTESIAN_POINT('Ctrl Pts',(-0.843383895613249,-0.0595300000000001,
-0.742736168477219));
#5280=CARTESIAN_POINT('',(-0.536443649899847,-0.05953,-0.987512846410683));
#5281=CARTESIAN_POINT('Origin',(0.,-0.05953,0.));
#5282=CARTESIAN_POINT('',(0.0548532617164172,-0.05953,-1.12247250791415));
#5283=CARTESIAN_POINT('Ctrl Pts',(-0.536443649899848,-0.0595300000000001,
-0.987512846410683));
#5284=CARTESIAN_POINT('Ctrl Pts',(-0.533501897135712,-0.0762225747374254,
-0.989110885965947));
#5285=CARTESIAN_POINT('Ctrl Pts',(-0.529268075276156,-0.0928409665394227,
-0.991396466802469));
#5286=CARTESIAN_POINT('Ctrl Pts',(-0.511762781179147,-0.144299303100741,
-1.00061845128527));
#5287=CARTESIAN_POINT('Ctrl Pts',(-0.493462957200432,-0.177024326825049,
-1.0099536580922));
#5288=CARTESIAN_POINT('Ctrl Pts',(-0.45280897844858,-0.227269801620063,
-1.02876878445619));
#5289=CARTESIAN_POINT('Ctrl Pts',(-0.425554672694337,-0.251265615809407,
-1.04048957871266));
#5290=CARTESIAN_POINT('Ctrl Pts',(-0.3787731215897,-0.279889827963178,-1.05829506364875));
#5291=CARTESIAN_POINT('Ctrl Pts',(-0.354166711873529,-0.290879136862659,
-1.06688848765783));
#5292=CARTESIAN_POINT('Ctrl Pts',(-0.302426893214944,-0.305251990234488,
-1.08269251410343));
#5293=CARTESIAN_POINT('Ctrl Pts',(-0.275287440920027,-0.308638795020976,
-1.0898803575765));
#5294=CARTESIAN_POINT('Ctrl Pts',(-0.224855950742601,-0.308638795020976,
-1.10139101611326));
#5295=CARTESIAN_POINT('Ctrl Pts',(-0.19728546073067,-0.305251990234488,
-1.10669035995599));
#5296=CARTESIAN_POINT('Ctrl Pts',(-0.143812384801039,-0.290879136862659,
-1.11490049012186));
#5297=CARTESIAN_POINT('Ctrl Pts',(-0.117914228755037,-0.279889827963178,
-1.1178344036749));
#5298=CARTESIAN_POINT('Ctrl Pts',(-0.0680399972366989,-0.251265615809407,
-1.12208997038458));
#5299=CARTESIAN_POINT('Ctrl Pts',(-0.0383992541984084,-0.227269801620063,
-1.12335509974011));
#5300=CARTESIAN_POINT('Ctrl Pts',(0.00639229239215326,-0.177024326825049,
-1.12404235695137));
#5301=CARTESIAN_POINT('Ctrl Pts',(0.0269302585198977,-0.144299303100741,
-1.12357162229597));
#5302=CARTESIAN_POINT('Ctrl Pts',(0.04670325263426,-0.0928409665394228,
-1.12285816383385));
#5303=CARTESIAN_POINT('Ctrl Pts',(0.0515094706813703,-0.0762225747374255,
-1.12263591311425));
#5304=CARTESIAN_POINT('Ctrl Pts',(0.0548532617164176,-0.0595300000000001,
-1.12247250791414));
#5305=CARTESIAN_POINT('',(0.437601487681057,-0.05953,-1.03511272300331));
#5306=CARTESIAN_POINT('Origin',(0.,-0.05953,0.));
#5307=CARTESIAN_POINT('',(0.911784794170997,-0.05953,-0.656964154625313));
#5308=CARTESIAN_POINT('Ctrl Pts',(0.437601487681056,-0.0595300000000001,
-1.03511272300331));
#5309=CARTESIAN_POINT('Ctrl Pts',(0.440685038163619,-0.0762225747374255,
-1.03380912944435));
#5310=CARTESIAN_POINT('Ctrl Pts',(0.445111721969657,-0.0928409665394228,
-1.03192403056628));
#5311=CARTESIAN_POINT('Ctrl Pts',(0.463236132117164,-0.144299303100741,
-1.0239876538093));
#5312=CARTESIAN_POINT('Ctrl Pts',(0.481944444320713,-0.177024326825049,
-1.01550068154148));
#5313=CARTESIAN_POINT('Ctrl Pts',(0.522002043615455,-0.227269801620064,
-0.995447160474328));
#5314=CARTESIAN_POINT('Ctrl Pts',(0.548158511259203,-0.251265615809407,
-0.981446681891443));
#5315=CARTESIAN_POINT('Ctrl Pts',(0.591247219971725,-0.279889827963178,
-0.955972930713954));
#5316=CARTESIAN_POINT('Ctrl Pts',(0.613307674922609,-0.290879136862659,
-0.942092777160053));
#5317=CARTESIAN_POINT('Ctrl Pts',(0.657923009631182,-0.305251990234487,
-0.91149460735272));
#5318=CARTESIAN_POINT('Ctrl Pts',(0.680463863683393,-0.308638795020976,
-0.894757676234429));
#5319=CARTESIAN_POINT('Ctrl Pts',(0.720906778729542,-0.308638795020976,
-0.862505527716294));
#5320=CARTESIAN_POINT('Ctrl Pts',(0.742239891936899,-0.305251990234488,
-0.844254137480381));
#5321=CARTESIAN_POINT('Ctrl Pts',(0.781998747691872,-0.290879136862659,
-0.80756613568454));
#5322=CARTESIAN_POINT('Ctrl Pts',(0.800439809856112,-0.279889827963178,
-0.789147407129765));
#5323=CARTESIAN_POINT('Ctrl Pts',(0.834863020612702,-0.251265615809407,
-0.752807465209441));
#5324=CARTESIAN_POINT('Ctrl Pts',(0.854332839576145,-0.227269801620064,
-0.73042219438957));
#5325=CARTESIAN_POINT('Ctrl Pts',(0.882797231409153,-0.177024326825049,
-0.695831250979106));
#5326=CARTESIAN_POINT('Ctrl Pts',(0.895234408667242,-0.144299303100741,
-0.679480524217551));
#5327=CARTESIAN_POINT('Ctrl Pts',(0.907004864562642,-0.0928409665394228,
-0.663576540841106));
#5328=CARTESIAN_POINT('Ctrl Pts',(0.909827729890942,-0.0762225747374256,
-0.659680317203144));
#5329=CARTESIAN_POINT('Ctrl Pts',(0.911784794170998,-0.0595300000000001,
-0.656964154625312));
#5330=CARTESIAN_POINT('',(1.08212377959455,-0.05953,-0.303251606722892));
#5331=CARTESIAN_POINT('Origin',(0.,-0.05953,0.));
#5332=CARTESIAN_POINT('',(1.08212377959455,-0.05953,0.303251606722892));
#5333=CARTESIAN_POINT('Ctrl Pts',(1.08212377959455,-0.0595300000000001,
-0.303251606722892));
#5334=CARTESIAN_POINT('Ctrl Pts',(1.0830271513892,-0.0762225747374255,-0.300028012588062));
#5335=CARTESIAN_POINT('Ctrl Pts',(1.08431331394788,-0.0928409665394228,
-0.2953917518996));
#5336=CARTESIAN_POINT('Ctrl Pts',(1.08940878963422,-0.144299303100741,-0.276273267473431));
#5337=CARTESIAN_POINT('Ctrl Pts',(1.09443784939331,-0.177024326825049,-0.256354979351213));
#5338=CARTESIAN_POINT('Ctrl Pts',(1.10373487993589,-0.227269801620064,-0.212533521233765));
#5339=CARTESIAN_POINT('Ctrl Pts',(1.10909715583869,-0.251265615809407,-0.183354415742157));
#5340=CARTESIAN_POINT('Ctrl Pts',(1.1160463456491,-0.279889827963178,-0.133783682657561));
#5341=CARTESIAN_POINT('Ctrl Pts',(1.11894887330541,-0.290879136862659,-0.107881990270302));
#5342=CARTESIAN_POINT('Ctrl Pts',(1.12284346704144,-0.305251990234488,-0.0539226701638766));
#5343=CARTESIAN_POINT('Ctrl Pts',(1.123812,-0.308638795020976,-0.025864214957475));
#5344=CARTESIAN_POINT('Ctrl Pts',(1.123812,-0.308638795020976,0.025864214957475));
#5345=CARTESIAN_POINT('Ctrl Pts',(1.12284346704144,-0.305251990234488,0.0539226701638766));
#5346=CARTESIAN_POINT('Ctrl Pts',(1.11894887330541,-0.290879136862659,0.107881990270302));
#5347=CARTESIAN_POINT('Ctrl Pts',(1.1160463456491,-0.279889827963178,0.133783682657561));
#5348=CARTESIAN_POINT('Ctrl Pts',(1.10909715583869,-0.251265615809407,0.183354415742157));
#5349=CARTESIAN_POINT('Ctrl Pts',(1.10373487993589,-0.227269801620064,0.212533521233765));
#5350=CARTESIAN_POINT('Ctrl Pts',(1.09443784939331,-0.177024326825049,0.256354979351213));
#5351=CARTESIAN_POINT('Ctrl Pts',(1.08940878963422,-0.144299303100741,0.276273267473431));
#5352=CARTESIAN_POINT('Ctrl Pts',(1.08431331394788,-0.0928409665394228,
0.2953917518996));
#5353=CARTESIAN_POINT('Ctrl Pts',(1.0830271513892,-0.0762225747374255,0.300028012588062));
#5354=CARTESIAN_POINT('Ctrl Pts',(1.08212377959455,-0.0595300000000001,
0.303251606722892));
#5355=CARTESIAN_POINT('Origin',(0.,-0.05953,0.));
#5356=CARTESIAN_POINT('Origin',(0.,-0.05953,0.));
#5357=CARTESIAN_POINT('',(0.0589974094846122,-0.05953,1.07456964270265));
#5358=CARTESIAN_POINT('Origin',(0.,-0.05953,0.));
#5359=CARTESIAN_POINT('Origin',(-0.244773027351946,-0.05953,1.07242070340001));
#5360=CARTESIAN_POINT('Origin',(-0.244773027351946,0.,1.07242070340001));
#5361=CARTESIAN_POINT('',(-0.519393123750572,-0.05953,0.942555777842682));
#5362=CARTESIAN_POINT('Ctrl Pts',(-0.519393123750572,-0.05953,0.942555777842682));
#5363=CARTESIAN_POINT('Ctrl Pts',(-0.513714466572041,-0.0925528133349865,
0.945684988399766));
#5364=CARTESIAN_POINT('Ctrl Pts',(-0.503136848051455,-0.124911173756694,
0.951483858396181));
#5365=CARTESIAN_POINT('Ctrl Pts',(-0.47593627990192,-0.177924977804098,
0.965323333309091));
#5366=CARTESIAN_POINT('Ctrl Pts',(-0.460931856495794,-0.199697230012983,
0.972669835243841));
#5367=CARTESIAN_POINT('Ctrl Pts',(-0.426157505475872,-0.237895043532788,
0.988400002689705));
#5368=CARTESIAN_POINT('Ctrl Pts',(-0.406380688682952,-0.254319232363049,
0.996771768218699));
#5369=CARTESIAN_POINT('Ctrl Pts',(-0.364750145543744,-0.28018331644634,
1.01272583306292));
#5370=CARTESIAN_POINT('Ctrl Pts',(-0.340838910881557,-0.29104845371857,
1.02112815447116));
#5371=CARTESIAN_POINT('Ctrl Pts',(-0.290495481564827,-0.30527573347708,
1.036574285215));
#5372=CARTESIAN_POINT('Ctrl Pts',(-0.264056468041074,-0.308638795020976,
1.04359501395068));
#5373=CARTESIAN_POINT('Ctrl Pts',(-0.214892249704082,-0.308638795020976,
1.05481642595959));
#5374=CARTESIAN_POINT('Ctrl Pts',(-0.188025341585962,-0.30527573347708,
1.05996242598502));
#5375=CARTESIAN_POINT('Ctrl Pts',(-0.135965654106109,-0.29104845371857,
1.06788913840721));
#5376=CARTESIAN_POINT('Ctrl Pts',(-0.110776745452494,-0.28018331644634,
1.07069360430242));
#5377=CARTESIAN_POINT('Ctrl Pts',(-0.0663467128214646,-0.254319232363049,
1.07438230428002));
#5378=CARTESIAN_POINT('Ctrl Pts',(-0.0448960436540983,-0.237895043532788,
1.07542044338697));
#5379=CARTESIAN_POINT('Ctrl Pts',(-0.00674037211528124,-0.199697230012983,
1.07633607767727));
#5380=CARTESIAN_POINT('Ctrl Pts',(0.00996567398334777,-0.177924977804098,
1.07622728347683));
#5381=CARTESIAN_POINT('Ctrl Pts',(0.0404772621979741,-0.124911173756694,
1.07556023164702));
#5382=CARTESIAN_POINT('Ctrl Pts',(0.0525234025782719,-0.0925528133349865,
1.07492508698591));
#5383=CARTESIAN_POINT('Ctrl Pts',(0.0589974094846124,-0.05953,1.07456964270265));
#5384=CARTESIAN_POINT('Origin',(-0.244773027351946,-0.05953,1.07242070340001));
#5385=CARTESIAN_POINT('Origin',(0.,-0.05953,0.));
#5386=CARTESIAN_POINT('',(-0.803348093619616,-0.05953,0.716109245731214));
#5387=CARTESIAN_POINT('Origin',(0.,-0.05953,0.));
#5388=CARTESIAN_POINT('Origin',(-0.991065754692661,-0.05953,0.477272113029314));
#5389=CARTESIAN_POINT('Origin',(-0.991065754692661,0.,0.477272113029314));
#5390=CARTESIAN_POINT('',(-1.06075609691358,-0.05953,0.181596019242328));
#5391=CARTESIAN_POINT('Ctrl Pts',(-1.06075609691358,-0.05953,0.181596019242328));
#5392=CARTESIAN_POINT('Ctrl Pts',(-1.05966202740332,-0.0925528133349865,
0.187986803072856));
#5393=CARTESIAN_POINT('Ctrl Pts',(-1.05760072925372,-0.124911173756694,
0.199872254546857));
#5394=CARTESIAN_POINT('Ctrl Pts',(-1.05146158959546,-0.177924977804098,
0.22976728653846));
#5395=CARTESIAN_POINT('Ctrl Pts',(-1.04785021111757,-0.199697230012983,
0.246078686169301));
#5396=CARTESIAN_POINT('Ctrl Pts',(-1.03846709802406,-0.237895043532788,
0.283073967563097));
#5397=CARTESIAN_POINT('Ctrl Pts',(-1.03268176429485,-0.254319232363049,
0.303755815985685));
#5398=CARTESIAN_POINT('Ctrl Pts',(-1.01919893537026,-0.28018331644634,0.346251081972725));
#5399=CARTESIAN_POINT('Ctrl Pts',(-1.01085972381132,-0.29104845371857,0.370184399726282));
#5400=CARTESIAN_POINT('Ctrl Pts',(-0.99154738033959,-0.30527573347708,0.419174982698463));
#5401=CARTESIAN_POINT('Ctrl Pts',(-0.980551951791748,-0.308638795020976,
0.444223188605045));
#5402=CARTESIAN_POINT('Ctrl Pts',(-0.958671816228589,-0.308638795020976,
0.489657758261848));
#5403=CARTESIAN_POINT('Ctrl Pts',(-0.945943877838127,-0.30527573347708,
0.51387163140139));
#5404=CARTESIAN_POINT('Ctrl Pts',(-0.91968254693063,-0.29104845371857,0.559515758398093));
#5405=CARTESIAN_POINT('Ctrl Pts',(-0.906170138993533,-0.28018331644634,
0.580957796077825));
#5406=CARTESIAN_POINT('Ctrl Pts',(-0.8813524085237,-0.254319232363049,0.617994461173994));
#5407=CARTESIAN_POINT('Ctrl Pts',(-0.868789784891799,-0.237895043532788,
0.635412538795143));
#5408=CARTESIAN_POINT('Ctrl Pts',(-0.845715984518854,-0.199697230012983,
0.66581473268113));
#5409=CARTESIAN_POINT('Ctrl Pts',(-0.835214876415962,-0.177924977804098,
0.678808213394124));
#5410=CARTESIAN_POINT('Ctrl Pts',(-0.815669690204649,-0.124911173756694,
0.702247233627224));
#5411=CARTESIAN_POINT('Ctrl Pts',(-0.807662468433796,-0.0925528133349865,
0.711269279199861));
#5412=CARTESIAN_POINT('Ctrl Pts',(-0.803348093619616,-0.05953,0.716109245731214));
#5413=CARTESIAN_POINT('Origin',(-0.991065754692661,-0.05953,0.477272113029314));
#5414=CARTESIAN_POINT('Origin',(0.,-0.05953,0.));
#5415=CARTESIAN_POINT('',(-1.076188,-0.05953,1.31795018948079E-16));
#5416=CARTESIAN_POINT('Origin',(0.,-0.05953,0.));
#5417=CARTESIAN_POINT('',(-1.06075609691358,-0.05953,-0.181596019242328));
#5418=CARTESIAN_POINT('Origin',(0.,-0.05953,0.));
#5419=CARTESIAN_POINT('Origin',(-0.991065754692661,-0.05953,-0.477272113029314));
#5420=CARTESIAN_POINT('Origin',(-0.991065754692661,0.,-0.477272113029314));
#5421=CARTESIAN_POINT('',(-0.803348093619616,-0.05953,-0.716109245731215));
#5422=CARTESIAN_POINT('Ctrl Pts',(-0.803348093619616,-0.05953,-0.716109245731215));
#5423=CARTESIAN_POINT('Ctrl Pts',(-0.807662468433795,-0.0925528133349865,
-0.711269279199862));
#5424=CARTESIAN_POINT('Ctrl Pts',(-0.815669690204649,-0.124911173756694,
-0.702247233627224));
#5425=CARTESIAN_POINT('Ctrl Pts',(-0.835214876415962,-0.177924977804098,
-0.678808213394124));
#5426=CARTESIAN_POINT('Ctrl Pts',(-0.845715984518854,-0.199697230012983,
-0.66581473268113));
#5427=CARTESIAN_POINT('Ctrl Pts',(-0.868789784891799,-0.237895043532788,
-0.635412538795143));
#5428=CARTESIAN_POINT('Ctrl Pts',(-0.8813524085237,-0.254319232363049,-0.617994461173994));
#5429=CARTESIAN_POINT('Ctrl Pts',(-0.906170138993533,-0.28018331644634,
-0.580957796077826));
#5430=CARTESIAN_POINT('Ctrl Pts',(-0.91968254693063,-0.29104845371857,-0.559515758398093));
#5431=CARTESIAN_POINT('Ctrl Pts',(-0.945943877838127,-0.30527573347708,
-0.51387163140139));
#5432=CARTESIAN_POINT('Ctrl Pts',(-0.958671816228589,-0.308638795020976,
-0.489657758261848));
#5433=CARTESIAN_POINT('Ctrl Pts',(-0.980551951791748,-0.308638795020976,
-0.444223188605045));
#5434=CARTESIAN_POINT('Ctrl Pts',(-0.99154738033959,-0.30527573347708,-0.419174982698463));
#5435=CARTESIAN_POINT('Ctrl Pts',(-1.01085972381132,-0.29104845371857,-0.370184399726282));
#5436=CARTESIAN_POINT('Ctrl Pts',(-1.01919893537026,-0.28018331644634,-0.346251081972725));
#5437=CARTESIAN_POINT('Ctrl Pts',(-1.03268176429485,-0.254319232363049,
-0.303755815985685));
#5438=CARTESIAN_POINT('Ctrl Pts',(-1.03846709802406,-0.237895043532788,
-0.283073967563097));
#5439=CARTESIAN_POINT('Ctrl Pts',(-1.04785021111757,-0.199697230012983,
-0.246078686169302));
#5440=CARTESIAN_POINT('Ctrl Pts',(-1.05146158959546,-0.177924977804098,
-0.229767286538461));
#5441=CARTESIAN_POINT('Ctrl Pts',(-1.05760072925372,-0.124911173756694,
-0.199872254546858));
#5442=CARTESIAN_POINT('Ctrl Pts',(-1.05966202740332,-0.0925528133349864,
-0.187986803072857));
#5443=CARTESIAN_POINT('Ctrl Pts',(-1.06075609691358,-0.05953,-0.181596019242328));
#5444=CARTESIAN_POINT('Origin',(-0.991065754692661,-0.05953,-0.477272113029314));
#5445=CARTESIAN_POINT('Origin',(0.,-0.05953,0.));
#5446=CARTESIAN_POINT('',(-0.519393123750572,-0.05953,-0.942555777842682));
#5447=CARTESIAN_POINT('Origin',(0.,-0.05953,0.));
#5448=CARTESIAN_POINT('Origin',(-0.244773027351946,-0.05953,-1.07242070340001));
#5449=CARTESIAN_POINT('Origin',(-0.244773027351946,0.,-1.07242070340001));
#5450=CARTESIAN_POINT('',(0.0589974094846125,-0.05953,-1.07456964270265));
#5451=CARTESIAN_POINT('Ctrl Pts',(0.0589974094846127,-0.05953,-1.07456964270265));
#5452=CARTESIAN_POINT('Ctrl Pts',(0.0525234025782722,-0.0925528133349865,
-1.07492508698591));
#5453=CARTESIAN_POINT('Ctrl Pts',(0.0404772621979744,-0.124911173756694,
-1.07556023164702));
#5454=CARTESIAN_POINT('Ctrl Pts',(0.0099656739833481,-0.177924977804098,
-1.07622728347683));
#5455=CARTESIAN_POINT('Ctrl Pts',(-0.00674037211528096,-0.199697230012983,
-1.07633607767727));
#5456=CARTESIAN_POINT('Ctrl Pts',(-0.044896043654098,-0.237895043532788,
-1.07542044338697));
#5457=CARTESIAN_POINT('Ctrl Pts',(-0.0663467128214644,-0.254319232363049,
-1.07438230428002));
#5458=CARTESIAN_POINT('Ctrl Pts',(-0.110776745452493,-0.28018331644634,
-1.07069360430242));
#5459=CARTESIAN_POINT('Ctrl Pts',(-0.135965654106109,-0.29104845371857,
-1.06788913840721));
#5460=CARTESIAN_POINT('Ctrl Pts',(-0.188025341585962,-0.30527573347708,
-1.05996242598502));
#5461=CARTESIAN_POINT('Ctrl Pts',(-0.214892249704082,-0.308638795020976,
-1.05481642595959));
#5462=CARTESIAN_POINT('Ctrl Pts',(-0.264056468041074,-0.308638795020976,
-1.04359501395068));
#5463=CARTESIAN_POINT('Ctrl Pts',(-0.290495481564827,-0.30527573347708,
-1.036574285215));
#5464=CARTESIAN_POINT('Ctrl Pts',(-0.340838910881557,-0.291048453718569,
-1.02112815447116));
#5465=CARTESIAN_POINT('Ctrl Pts',(-0.364750145543744,-0.28018331644634,
-1.01272583306292));
#5466=CARTESIAN_POINT('Ctrl Pts',(-0.406380688682952,-0.254319232363049,
-0.996771768218699));
#5467=CARTESIAN_POINT('Ctrl Pts',(-0.426157505475872,-0.237895043532788,
-0.988400002689705));
#5468=CARTESIAN_POINT('Ctrl Pts',(-0.460931856495794,-0.199697230012983,
-0.972669835243841));
#5469=CARTESIAN_POINT('Ctrl Pts',(-0.475936279901919,-0.177924977804098,
-0.965323333309091));
#5470=CARTESIAN_POINT('Ctrl Pts',(-0.503136848051454,-0.124911173756694,
-0.951483858396181));
#5471=CARTESIAN_POINT('Ctrl Pts',(-0.513714466572041,-0.0925528133349865,
-0.945684988399766));
#5472=CARTESIAN_POINT('Ctrl Pts',(-0.519393123750572,-0.05953,-0.942555777842682));
#5473=CARTESIAN_POINT('Origin',(-0.244773027351946,-0.05953,-1.07242070340001));
#5474=CARTESIAN_POINT('Origin',(0.,-0.05953,0.));
#5475=CARTESIAN_POINT('',(0.413083465285518,-0.05953,-0.993751811093549));
#5476=CARTESIAN_POINT('Origin',(0.,-0.05953,0.));
#5477=CARTESIAN_POINT('Origin',(0.685838782044607,-0.05953,-0.860014630714833));
#5478=CARTESIAN_POINT('Origin',(0.685838782044607,0.,-0.860014630714833));
#5479=CARTESIAN_POINT('',(0.876916659919095,-0.05953,-0.623857181492959));
#5480=CARTESIAN_POINT('Ctrl Pts',(0.876916659919095,-0.05953,-0.623857181492958));
#5481=CARTESIAN_POINT('Ctrl Pts',(0.873158080166742,-0.0925528133349865,
-0.62914037979579));
#5482=CARTESIAN_POINT('Ctrl Pts',(0.866144010579847,-0.124911173756694,
-0.638954437806245));
#5483=CARTESIAN_POINT('Ctrl Pts',(0.847641868610495,-0.177924977804098,
-0.663225258065736));
#5484=CARTESIAN_POINT('Ctrl Pts',(0.837310877969633,-0.199697230012983,
-0.676354402927683));
#5485=CARTESIAN_POINT('Ctrl Pts',(0.81280533416753,-0.237895043532788,-0.705614819529209));
#5486=CARTESIAN_POINT('Ctrl Pts',(0.798619410861634,-0.254319232363049,
-0.721738358858166));
#5487=CARTESIAN_POINT('Ctrl Pts',(0.768033796848072,-0.28018331644634,-0.754175290318038));
#5488=CARTESIAN_POINT('Ctrl Pts',(0.750136149454208,-0.29104845371857,-0.772120216227122));
#5489=CARTESIAN_POINT('Ctrl Pts',(0.711480111898423,-0.30527573347708,-0.807879894508811));
#5490=CARTESIAN_POINT('Ctrl Pts',(0.690705563850638,-0.308638795020976,
-0.825676810575913));
#5491=CARTESIAN_POINT('Ctrl Pts',(0.651278921914856,-0.308638795020976,
-0.857118508332695));
#5492=CARTESIAN_POINT('Ctrl Pts',(0.629305439856167,-0.30527573347708,-0.873412008702649));
#5493=CARTESIAN_POINT('Ctrl Pts',(0.585840553788742,-0.29104845371857,-0.903141581680914));
#5494=CARTESIAN_POINT('Ctrl Pts',(0.564362943424239,-0.28018331644634,-0.916597376014514));
#5495=CARTESIAN_POINT('Ctrl Pts',(0.525933334162556,-0.254319232363049,
-0.939198248544427));
#5496=CARTESIAN_POINT('Ctrl Pts',(0.507057380724533,-0.237895043532788,
-0.949440676105255));
#5497=CARTESIAN_POINT('Ctrl Pts',(0.473077587363686,-0.199697230012983,
-0.966820759530997));
#5498=CARTESIAN_POINT('Ctrl Pts',(0.457978755888596,-0.177924977804098,
-0.973971221090534));
#5499=CARTESIAN_POINT('Ctrl Pts',(0.430199341854858,-0.124911173756694,
-0.986608710139579));
#5500=CARTESIAN_POINT('Ctrl Pts',(0.419070565453384,-0.0925528133349865,
-0.991263089003441));
#5501=CARTESIAN_POINT('Ctrl Pts',(0.413083465285518,-0.05953,-0.993751811093549));
#5502=CARTESIAN_POINT('Origin',(0.685838782044607,-0.05953,-0.860014630714833));
#5503=CARTESIAN_POINT('Origin',(0.,-0.208355,0.));
#5504=CARTESIAN_POINT('',(-1.076188,-0.35718,1.31795018948079E-16));
#5505=CARTESIAN_POINT('Origin',(0.,-0.35718,0.));
#5506=CARTESIAN_POINT('',(-1.076188,-0.208355,1.31795018948079E-16));
#5507=CARTESIAN_POINT('',(1.03449977959455,-0.05953,0.296632461748266));
#5508=CARTESIAN_POINT('Origin',(0.,-0.05953,0.));
#5509=CARTESIAN_POINT('',(1.03449977959455,-0.05953,-0.296632461748266));
#5510=CARTESIAN_POINT('Ctrl Pts',(1.03449977959455,-0.05953,0.296632461748267));
#5511=CARTESIAN_POINT('Ctrl Pts',(1.03628691421076,-0.0925528133349865,
0.290399865505497));
#5512=CARTESIAN_POINT('Ctrl Pts',(1.03958665287714,-0.124911173756694,0.278797079997872));
#5513=CARTESIAN_POINT('Ctrl Pts',(1.0470264474309,-0.177924977804098,0.249198913998601));
#5514=CARTESIAN_POINT('Ctrl Pts',(1.05084995891418,-0.199697230012983,0.232935932341942));
#5515=CARTESIAN_POINT('Ctrl Pts',(1.05844771715377,-0.237895043532788,0.195533155353269));
#5516=CARTESIAN_POINT('Ctrl Pts',(1.06220882929878,-0.254319232363049,0.17438929156337));
#5517=CARTESIAN_POINT('Ctrl Pts',(1.06849922508772,-0.28018331644634,0.130252399648131));
#5518=CARTESIAN_POINT('Ctrl Pts',(1.07137013248666,-0.29104845371857,0.105070977154072));
#5519=CARTESIAN_POINT('Ctrl Pts',(1.07522652957392,-0.30527573347708,0.0525526752791107));
#5520=CARTESIAN_POINT('Ctrl Pts',(1.076188,-0.308638795020976,0.025214283908933));
#5521=CARTESIAN_POINT('Ctrl Pts',(1.076188,-0.308638795020976,-0.025214283908933));
#5522=CARTESIAN_POINT('Ctrl Pts',(1.07522652957392,-0.30527573347708,-0.0525526752791107));
#5523=CARTESIAN_POINT('Ctrl Pts',(1.07137013248666,-0.29104845371857,-0.105070977154072));
#5524=CARTESIAN_POINT('Ctrl Pts',(1.06849922508772,-0.28018331644634,-0.130252399648131));
#5525=CARTESIAN_POINT('Ctrl Pts',(1.06220882929878,-0.254319232363049,-0.17438929156337));
#5526=CARTESIAN_POINT('Ctrl Pts',(1.05844771715377,-0.237895043532788,-0.195533155353269));
#5527=CARTESIAN_POINT('Ctrl Pts',(1.05084995891418,-0.199697230012983,-0.232935932341942));
#5528=CARTESIAN_POINT('Ctrl Pts',(1.0470264474309,-0.177924977804098,-0.249198913998601));
#5529=CARTESIAN_POINT('Ctrl Pts',(1.03958665287714,-0.124911173756694,-0.278797079997872));
#5530=CARTESIAN_POINT('Ctrl Pts',(1.03628691421076,-0.0925528133349865,
-0.290399865505497));
#5531=CARTESIAN_POINT('Ctrl Pts',(1.03449977959455,-0.05953,-0.296632461748267));
#5532=CARTESIAN_POINT('Origin',(0.,-0.05953,0.));
#5533=CARTESIAN_POINT('Origin',(0.,-0.05953,0.));
#5534=CARTESIAN_POINT('Origin',(1.1,-0.05953,0.));
#5535=CARTESIAN_POINT('Origin',(1.1,0.,0.));
#5536=CARTESIAN_POINT('Origin',(1.1,-0.05953,0.));
#5537=CARTESIAN_POINT('Origin',(0.,-0.35718,0.));
#5538=CARTESIAN_POINT('Origin',(0.,-0.05953,0.));
#5539=CARTESIAN_POINT('',(0.,0.,0.));
#5540=CARTESIAN_POINT('Origin',(1.119765,0.495,0.));
#5541=CARTESIAN_POINT('',(-1.119765,0.495,-1.37131662304724E-16));
#5542=CARTESIAN_POINT('Origin',(0.,0.495,0.));
#5543=CARTESIAN_POINT('',(-1.085235,0.495,-1.32902956907268E-16));
#5544=CARTESIAN_POINT('Origin',(0.,0.495,0.));
#5545=CARTESIAN_POINT('Origin',(0.,0.4575,0.));
#5546=CARTESIAN_POINT('',(-1.119765,0.42,-1.37131662304724E-16));
#5547=CARTESIAN_POINT('Origin',(0.,0.42,0.));
#5548=CARTESIAN_POINT('',(-1.119765,0.4575,-1.37131662304724E-16));
#5549=CARTESIAN_POINT('Origin',(1.085235,0.42,0.));
#5550=CARTESIAN_POINT('',(-1.085235,0.42,-1.32902956907268E-16));
#5551=CARTESIAN_POINT('Origin',(0.,0.42,0.));
#5552=CARTESIAN_POINT('Origin',(0.,0.4575,0.));
#5553=CARTESIAN_POINT('',(-1.085235,0.4575,-1.32902956907268E-16));
#5554=CARTESIAN_POINT('Origin',(1.119765,-0.42,0.));
#5555=CARTESIAN_POINT('',(-1.119765,-0.42,-1.37131662304724E-16));
#5556=CARTESIAN_POINT('Origin',(0.,-0.42,0.));
#5557=CARTESIAN_POINT('',(-1.085235,-0.42,-1.32902956907268E-16));
#5558=CARTESIAN_POINT('Origin',(0.,-0.42,0.));
#5559=CARTESIAN_POINT('Origin',(0.,-0.4575,0.));
#5560=CARTESIAN_POINT('',(-1.119765,-0.495,-1.37131662304724E-16));
#5561=CARTESIAN_POINT('Origin',(0.,-0.495,0.));
#5562=CARTESIAN_POINT('',(-1.119765,-0.4575,-1.37131662304724E-16));
#5563=CARTESIAN_POINT('Origin',(1.085235,-0.495,0.));
#5564=CARTESIAN_POINT('',(-1.085235,-0.495,-1.32902956907268E-16));
#5565=CARTESIAN_POINT('Origin',(0.,-0.495,0.));
#5566=CARTESIAN_POINT('Origin',(0.,-0.4575,0.));
#5567=CARTESIAN_POINT('',(-1.085235,-0.4575,-1.32902956907268E-16));
#5568=CARTESIAN_POINT('',(0.,0.,0.));
#5569=CARTESIAN_POINT('',(0.,0.,0.));
#5570=CARTESIAN_POINT('',(0.,0.,0.));
#5571=CARTESIAN_POINT('',(0.,0.,0.));
#5572=CARTESIAN_POINT('',(0.,0.,0.));
#5573=CARTESIAN_POINT('',(0.,0.,0.));
#5574=CARTESIAN_POINT('Origin',(0.,1.1,3.5));
#5575=CARTESIAN_POINT('',(-1.2,1.3,3.5));
#5576=CARTESIAN_POINT('Origin',(0.,1.3,3.5));
#5577=CARTESIAN_POINT('',(-1.2,1.1,3.5));
#5578=CARTESIAN_POINT('',(-1.2,1.1,3.5));
#5579=CARTESIAN_POINT('Origin',(0.,1.1,3.5));
#5580=CARTESIAN_POINT('Origin',(0.,1.1,3.5));
#5581=CARTESIAN_POINT('',(-1.6,1.3,3.5));
#5582=CARTESIAN_POINT('Origin',(0.,1.3,3.5));
#5583=CARTESIAN_POINT('',(-1.6,1.1,3.5));
#5584=CARTESIAN_POINT('',(-1.6,1.1,3.5));
#5585=CARTESIAN_POINT('Origin',(0.,1.1,3.5));
#5586=CARTESIAN_POINT('Origin',(0.,1.3,3.5));
#5587=CARTESIAN_POINT('Origin',(0.,1.1,3.5));
#5588=CARTESIAN_POINT('',(0.,0.,1.));
#5589=CARTESIAN_POINT('',(0.,-0.6,5.));
#5590=CARTESIAN_POINT('',(0.,0.6,5.));
#5591=CARTESIAN_POINT('',(0.,0.,1.5));
#5592=CARTESIAN_POINT('',(0.,-2.4,1.5));
#5593=CARTESIAN_POINT('',(0.,0.,0.));
#5594=CARTESIAN_POINT('',(0.,0.,0.));
#5595=CARTESIAN_POINT('Origin',(-3.,-0.7,9.));
#5596=CARTESIAN_POINT('',(-3.325,-0.6,9.));
#5597=CARTESIAN_POINT('Origin',(-3.,-0.6,9.));
#5598=CARTESIAN_POINT('',(-3.325,0.6,9.));
#5599=CARTESIAN_POINT('',(-3.325,-0.7,9.));
#5600=CARTESIAN_POINT('Origin',(-3.,0.6,9.));
#5601=CARTESIAN_POINT('Origin',(-6.5,-0.6,8.6));
#5602=CARTESIAN_POINT('',(-3.57047275484513,0.6,9.18590544903097));
#5603=CARTESIAN_POINT('',(-3.57047275484513,-0.6,9.18590544903098));
#5604=CARTESIAN_POINT('',(-3.57047275484513,-0.6,9.18590544903097));
#5605=CARTESIAN_POINT('',(-6.5,0.6,8.6));
#5606=CARTESIAN_POINT('',(-3.,0.6,9.3));
#5607=CARTESIAN_POINT('',(-6.5,-0.6,8.6));
#5608=CARTESIAN_POINT('',(-6.5,-0.6,8.6));
#5609=CARTESIAN_POINT('',(-3.,-0.6,9.3));
#5610=CARTESIAN_POINT('Origin',(-6.5,-0.6,8.));
#5611=CARTESIAN_POINT('',(-6.5,-0.6,8.));
#5612=CARTESIAN_POINT('',(-6.5,-0.6,8.6));
#5613=CARTESIAN_POINT('',(-6.5,0.6,8.));
#5614=CARTESIAN_POINT('',(-6.5,0.6,8.6));
#5615=CARTESIAN_POINT('',(-6.5,-0.6,8.));
#5616=CARTESIAN_POINT('Origin',(-3.,-0.6,8.7));
#5617=CARTESIAN_POINT('',(-3.45508813946051,-0.6,8.6089823721079));
#5618=CARTESIAN_POINT('',(-3.45508813946051,0.6,8.6089823721079));
#5619=CARTESIAN_POINT('',(-3.45508813946051,-0.6,8.6089823721079));
#5620=CARTESIAN_POINT('',(-6.5,-0.6,8.));
#5621=CARTESIAN_POINT('',(-6.5,0.6,8.));
#5622=CARTESIAN_POINT('Origin',(-3.,-0.6,9.));
#5623=CARTESIAN_POINT('',(-2.48038475772934,-0.6,9.3));
#5624=CARTESIAN_POINT('Origin',(-3.,-0.6,9.));
#5625=CARTESIAN_POINT('',(0.5,-0.6,9.3));
#5626=CARTESIAN_POINT('',(-3.,-0.6,9.3));
#5627=CARTESIAN_POINT('',(0.5,-0.6,9.9));
#5628=CARTESIAN_POINT('',(0.5,-0.6,9.3));
#5629=CARTESIAN_POINT('',(-3.,-0.6,9.9));
#5630=CARTESIAN_POINT('',(0.5,-0.6,9.9));
#5631=CARTESIAN_POINT('',(-3.,-0.6,9.6));
#5632=CARTESIAN_POINT('',(-3.,-0.6,9.9));
#5633=CARTESIAN_POINT('Origin',(-3.,-0.6,9.));
#5634=CARTESIAN_POINT('Origin',(-3.,-0.6,9.));
#5635=CARTESIAN_POINT('',(-2.48038475772934,0.6,9.3));
#5636=CARTESIAN_POINT('Origin',(-3.,0.6,9.));
#5637=CARTESIAN_POINT('',(-2.48038475772934,-0.6,9.3));
#5638=CARTESIAN_POINT('Origin',(-3.,-0.6,9.3));
#5639=CARTESIAN_POINT('',(-3.,0.6,9.6));
#5640=CARTESIAN_POINT('',(-3.,-0.6,9.6));
#5641=CARTESIAN_POINT('',(-3.,0.6,9.9));
#5642=CARTESIAN_POINT('',(-3.,-0.6,9.9));
#5643=CARTESIAN_POINT('',(-3.,0.6,9.9));
#5644=CARTESIAN_POINT('Origin',(0.5,-0.6,9.3));
#5645=CARTESIAN_POINT('',(0.5,0.6,9.3));
#5646=CARTESIAN_POINT('',(-3.,0.6,9.3));
#5647=CARTESIAN_POINT('',(0.5,-0.6,9.3));
#5648=CARTESIAN_POINT('Origin',(0.5,-0.6,9.9));
#5649=CARTESIAN_POINT('',(0.5,0.6,9.9));
#5650=CARTESIAN_POINT('',(0.5,0.6,9.3));
#5651=CARTESIAN_POINT('',(0.5,-0.6,9.9));
#5652=CARTESIAN_POINT('Origin',(-3.,-0.6,9.9));
#5653=CARTESIAN_POINT('',(0.5,0.6,9.9));
#5654=CARTESIAN_POINT('Origin',(-3.,0.6,9.));
#5655=CARTESIAN_POINT('Origin',(-3.,0.6,9.));
#5656=CARTESIAN_POINT('Origin',(-3.,-0.6,9.));
#5657=CARTESIAN_POINT('',(0.,0.,0.));
#5658=CARTESIAN_POINT('Origin',(0.5,0.6,8.75));
#5659=CARTESIAN_POINT('',(0.5,0.6,8.75));
#5660=CARTESIAN_POINT('',(-0.5,0.6,8.75));
#5661=CARTESIAN_POINT('',(0.5,0.6,8.75));
#5662=CARTESIAN_POINT('',(-0.5,0.6,9.3));
#5663=CARTESIAN_POINT('',(-0.5,0.6,8.75));
#5664=CARTESIAN_POINT('',(0.5,0.6,9.3));
#5665=CARTESIAN_POINT('',(0.5,0.6,9.3));
#5666=CARTESIAN_POINT('',(0.5,0.6,8.75));
#5667=CARTESIAN_POINT('Origin',(0.5,-0.6,8.75));
#5668=CARTESIAN_POINT('',(0.5,-0.6,8.75));
#5669=CARTESIAN_POINT('',(0.5,-0.6,8.75));
#5670=CARTESIAN_POINT('',(0.5,-0.6,9.3));
#5671=CARTESIAN_POINT('',(0.5,-0.6,9.3));
#5672=CARTESIAN_POINT('',(0.5,-0.6,8.75));
#5673=CARTESIAN_POINT('Origin',(-0.5,-0.6,8.75));
#5674=CARTESIAN_POINT('',(-0.5,-0.6,8.75));
#5675=CARTESIAN_POINT('',(-0.5,-0.6,8.75));
#5676=CARTESIAN_POINT('',(-0.5,-0.6,9.3));
#5677=CARTESIAN_POINT('',(-0.5,-0.6,9.3));
#5678=CARTESIAN_POINT('',(-0.5,-0.6,8.75));
#5679=CARTESIAN_POINT('Origin',(-0.5,0.6,8.75));
#5680=CARTESIAN_POINT('',(-0.5,0.6,8.75));
#5681=CARTESIAN_POINT('',(-0.5,0.6,9.3));
#5682=CARTESIAN_POINT('Origin',(0.,0.,9.3));
#5683=CARTESIAN_POINT('Origin',(0.,0.,8.75));
#5684=CARTESIAN_POINT('',(0.,0.,0.));
#5685=CARTESIAN_POINT('',(0.,0.,0.));
#5686=CARTESIAN_POINT('',(0.,0.,0.));
#5687=CARTESIAN_POINT('',(0.,0.,0.));
#5688=CARTESIAN_POINT('',(0.,0.,0.));
#5689=UNCERTAINTY_MEASURE_WITH_UNIT(LENGTH_MEASURE(0.001),#5735,
'DISTANCE_ACCURACY_VALUE',
'Maximum model space distance between geometric entities at asserted c
onnectivities');
#5690=UNCERTAINTY_MEASURE_WITH_UNIT(LENGTH_MEASURE(0.001),#5735,
'DISTANCE_ACCURACY_VALUE',
'Maximum model space distance between geometric entities at asserted c
onnectivities');
#5691=UNCERTAINTY_MEASURE_WITH_UNIT(LENGTH_MEASURE(0.001),#5735,
'DISTANCE_ACCURACY_VALUE',
'Maximum model space distance between geometric entities at asserted c
onnectivities');
#5692=UNCERTAINTY_MEASURE_WITH_UNIT(LENGTH_MEASURE(0.001),#5735,
'DISTANCE_ACCURACY_VALUE',
'Maximum model space distance between geometric entities at asserted c
onnectivities');
#5693=UNCERTAINTY_MEASURE_WITH_UNIT(LENGTH_MEASURE(0.001),#5735,
'DISTANCE_ACCURACY_VALUE',
'Maximum model space distance between geometric entities at asserted c
onnectivities');
#5694=UNCERTAINTY_MEASURE_WITH_UNIT(LENGTH_MEASURE(0.001),#5735,
'DISTANCE_ACCURACY_VALUE',
'Maximum model space distance between geometric entities at asserted c
onnectivities');
#5695=UNCERTAINTY_MEASURE_WITH_UNIT(LENGTH_MEASURE(0.001),#5735,
'DISTANCE_ACCURACY_VALUE',
'Maximum model space distance between geometric entities at asserted c
onnectivities');
#5696=UNCERTAINTY_MEASURE_WITH_UNIT(LENGTH_MEASURE(0.001),#5735,
'DISTANCE_ACCURACY_VALUE',
'Maximum model space distance between geometric entities at asserted c
onnectivities');
#5697=UNCERTAINTY_MEASURE_WITH_UNIT(LENGTH_MEASURE(0.001),#5735,
'DISTANCE_ACCURACY_VALUE',
'Maximum model space distance between geometric entities at asserted c
onnectivities');
#5698=UNCERTAINTY_MEASURE_WITH_UNIT(LENGTH_MEASURE(0.001),#5735,
'DISTANCE_ACCURACY_VALUE',
'Maximum model space distance between geometric entities at asserted c
onnectivities');
#5699=UNCERTAINTY_MEASURE_WITH_UNIT(LENGTH_MEASURE(0.001),#5735,
'DISTANCE_ACCURACY_VALUE',
'Maximum model space distance between geometric entities at asserted c
onnectivities');
#5700=UNCERTAINTY_MEASURE_WITH_UNIT(LENGTH_MEASURE(0.001),#5735,
'DISTANCE_ACCURACY_VALUE',
'Maximum model space distance between geometric entities at asserted c
onnectivities');
#5701=UNCERTAINTY_MEASURE_WITH_UNIT(LENGTH_MEASURE(0.001),#5735,
'DISTANCE_ACCURACY_VALUE',
'Maximum model space distance between geometric entities at asserted c
onnectivities');
#5702=UNCERTAINTY_MEASURE_WITH_UNIT(LENGTH_MEASURE(0.001),#5735,
'DISTANCE_ACCURACY_VALUE',
'Maximum model space distance between geometric entities at asserted c
onnectivities');
#5703=UNCERTAINTY_MEASURE_WITH_UNIT(LENGTH_MEASURE(0.001),#5735,
'DISTANCE_ACCURACY_VALUE',
'Maximum model space distance between geometric entities at asserted c
onnectivities');
#5704=UNCERTAINTY_MEASURE_WITH_UNIT(LENGTH_MEASURE(0.001),#5735,
'DISTANCE_ACCURACY_VALUE',
'Maximum model space distance between geometric entities at asserted c
onnectivities');
#5705=UNCERTAINTY_MEASURE_WITH_UNIT(LENGTH_MEASURE(0.001),#5735,
'DISTANCE_ACCURACY_VALUE',
'Maximum model space distance between geometric entities at asserted c
onnectivities');
#5706=UNCERTAINTY_MEASURE_WITH_UNIT(LENGTH_MEASURE(0.001),#5735,
'DISTANCE_ACCURACY_VALUE',
'Maximum model space distance between geometric entities at asserted c
onnectivities');
#5707=UNCERTAINTY_MEASURE_WITH_UNIT(LENGTH_MEASURE(0.001),#5735,
'DISTANCE_ACCURACY_VALUE',
'Maximum model space distance between geometric entities at asserted c
onnectivities');
#5708=UNCERTAINTY_MEASURE_WITH_UNIT(LENGTH_MEASURE(0.001),#5735,
'DISTANCE_ACCURACY_VALUE',
'Maximum model space distance between geometric entities at asserted c
onnectivities');
#5709=UNCERTAINTY_MEASURE_WITH_UNIT(LENGTH_MEASURE(0.001),#5735,
'DISTANCE_ACCURACY_VALUE',
'Maximum model space distance between geometric entities at asserted c
onnectivities');
#5710=UNCERTAINTY_MEASURE_WITH_UNIT(LENGTH_MEASURE(0.001),#5735,
'DISTANCE_ACCURACY_VALUE',
'Maximum model space distance between geometric entities at asserted c
onnectivities');
#5711=UNCERTAINTY_MEASURE_WITH_UNIT(LENGTH_MEASURE(0.001),#5735,
'DISTANCE_ACCURACY_VALUE',
'Maximum model space distance between geometric entities at asserted c
onnectivities');
#5712=(
GEOMETRIC_REPRESENTATION_CONTEXT(3)
GLOBAL_UNCERTAINTY_ASSIGNED_CONTEXT((#5689))
GLOBAL_UNIT_ASSIGNED_CONTEXT((#5735,#5737,#5738))
REPRESENTATION_CONTEXT('','3D')
);
#5713=(
GEOMETRIC_REPRESENTATION_CONTEXT(3)
GLOBAL_UNCERTAINTY_ASSIGNED_CONTEXT((#5690))
GLOBAL_UNIT_ASSIGNED_CONTEXT((#5735,#5737,#5738))
REPRESENTATION_CONTEXT('','3D')
);
#5714=(
GEOMETRIC_REPRESENTATION_CONTEXT(3)
GLOBAL_UNCERTAINTY_ASSIGNED_CONTEXT((#5691))
GLOBAL_UNIT_ASSIGNED_CONTEXT((#5735,#5737,#5738))
REPRESENTATION_CONTEXT('','3D')
);
#5715=(
GEOMETRIC_REPRESENTATION_CONTEXT(3)
GLOBAL_UNCERTAINTY_ASSIGNED_CONTEXT((#5692))
GLOBAL_UNIT_ASSIGNED_CONTEXT((#5735,#5737,#5738))
REPRESENTATION_CONTEXT('','3D')
);
#5716=(
GEOMETRIC_REPRESENTATION_CONTEXT(3)
GLOBAL_UNCERTAINTY_ASSIGNED_CONTEXT((#5693))
GLOBAL_UNIT_ASSIGNED_CONTEXT((#5735,#5737,#5738))
REPRESENTATION_CONTEXT('','3D')
);
#5717=(
GEOMETRIC_REPRESENTATION_CONTEXT(3)
GLOBAL_UNCERTAINTY_ASSIGNED_CONTEXT((#5694))
GLOBAL_UNIT_ASSIGNED_CONTEXT((#5735,#5737,#5738))
REPRESENTATION_CONTEXT('','3D')
);
#5718=(
GEOMETRIC_REPRESENTATION_CONTEXT(3)
GLOBAL_UNCERTAINTY_ASSIGNED_CONTEXT((#5695))
GLOBAL_UNIT_ASSIGNED_CONTEXT((#5735,#5737,#5738))
REPRESENTATION_CONTEXT('','3D')
);
#5719=(
GEOMETRIC_REPRESENTATION_CONTEXT(3)
GLOBAL_UNCERTAINTY_ASSIGNED_CONTEXT((#5696))
GLOBAL_UNIT_ASSIGNED_CONTEXT((#5735,#5737,#5738))
REPRESENTATION_CONTEXT('','3D')
);
#5720=(
GEOMETRIC_REPRESENTATION_CONTEXT(3)
GLOBAL_UNCERTAINTY_ASSIGNED_CONTEXT((#5697))
GLOBAL_UNIT_ASSIGNED_CONTEXT((#5735,#5737,#5738))
REPRESENTATION_CONTEXT('','3D')
);
#5721=(
GEOMETRIC_REPRESENTATION_CONTEXT(3)
GLOBAL_UNCERTAINTY_ASSIGNED_CONTEXT((#5698))
GLOBAL_UNIT_ASSIGNED_CONTEXT((#5735,#5737,#5738))
REPRESENTATION_CONTEXT('','3D')
);
#5722=(
GEOMETRIC_REPRESENTATION_CONTEXT(3)
GLOBAL_UNCERTAINTY_ASSIGNED_CONTEXT((#5699))
GLOBAL_UNIT_ASSIGNED_CONTEXT((#5735,#5737,#5738))
REPRESENTATION_CONTEXT('','3D')
);
#5723=(
GEOMETRIC_REPRESENTATION_CONTEXT(3)
GLOBAL_UNCERTAINTY_ASSIGNED_CONTEXT((#5700))
GLOBAL_UNIT_ASSIGNED_CONTEXT((#5735,#5737,#5738))
REPRESENTATION_CONTEXT('','3D')
);
#5724=(
GEOMETRIC_REPRESENTATION_CONTEXT(3)
GLOBAL_UNCERTAINTY_ASSIGNED_CONTEXT((#5701))
GLOBAL_UNIT_ASSIGNED_CONTEXT((#5735,#5737,#5738))
REPRESENTATION_CONTEXT('','3D')
);
#5725=(
GEOMETRIC_REPRESENTATION_CONTEXT(3)
GLOBAL_UNCERTAINTY_ASSIGNED_CONTEXT((#5702))
GLOBAL_UNIT_ASSIGNED_CONTEXT((#5735,#5737,#5738))
REPRESENTATION_CONTEXT('','3D')
);
#5726=(
GEOMETRIC_REPRESENTATION_CONTEXT(3)
GLOBAL_UNCERTAINTY_ASSIGNED_CONTEXT((#5703))
GLOBAL_UNIT_ASSIGNED_CONTEXT((#5735,#5737,#5738))
REPRESENTATION_CONTEXT('','3D')
);
#5727=(
GEOMETRIC_REPRESENTATION_CONTEXT(3)
GLOBAL_UNCERTAINTY_ASSIGNED_CONTEXT((#5704))
GLOBAL_UNIT_ASSIGNED_CONTEXT((#5735,#5737,#5738))
REPRESENTATION_CONTEXT('','3D')
);
#5728=(
GEOMETRIC_REPRESENTATION_CONTEXT(3)
GLOBAL_UNCERTAINTY_ASSIGNED_CONTEXT((#5705))
GLOBAL_UNIT_ASSIGNED_CONTEXT((#5735,#5737,#5738))
REPRESENTATION_CONTEXT('','3D')
);
#5729=(
GEOMETRIC_REPRESENTATION_CONTEXT(3)
GLOBAL_UNCERTAINTY_ASSIGNED_CONTEXT((#5706))
GLOBAL_UNIT_ASSIGNED_CONTEXT((#5735,#5737,#5738))
REPRESENTATION_CONTEXT('','3D')
);
#5730=(
GEOMETRIC_REPRESENTATION_CONTEXT(3)
GLOBAL_UNCERTAINTY_ASSIGNED_CONTEXT((#5707))
GLOBAL_UNIT_ASSIGNED_CONTEXT((#5735,#5737,#5738))
REPRESENTATION_CONTEXT('','3D')
);
#5731=(
GEOMETRIC_REPRESENTATION_CONTEXT(3)
GLOBAL_UNCERTAINTY_ASSIGNED_CONTEXT((#5708))
GLOBAL_UNIT_ASSIGNED_CONTEXT((#5735,#5737,#5738))
REPRESENTATION_CONTEXT('','3D')
);
#5732=(
GEOMETRIC_REPRESENTATION_CONTEXT(3)
GLOBAL_UNCERTAINTY_ASSIGNED_CONTEXT((#5709))
GLOBAL_UNIT_ASSIGNED_CONTEXT((#5735,#5737,#5738))
REPRESENTATION_CONTEXT('','3D')
);
#5733=(
GEOMETRIC_REPRESENTATION_CONTEXT(3)
GLOBAL_UNCERTAINTY_ASSIGNED_CONTEXT((#5710))
GLOBAL_UNIT_ASSIGNED_CONTEXT((#5735,#5737,#5738))
REPRESENTATION_CONTEXT('','3D')
);
#5734=(
GEOMETRIC_REPRESENTATION_CONTEXT(3)
GLOBAL_UNCERTAINTY_ASSIGNED_CONTEXT((#5711))
GLOBAL_UNIT_ASSIGNED_CONTEXT((#5735,#5737,#5738))
REPRESENTATION_CONTEXT('','3D')
);
#5735=(
LENGTH_UNIT()
NAMED_UNIT(*)
SI_UNIT(.CENTI.,.METRE.)
);
#5736=(
LENGTH_UNIT()
NAMED_UNIT(*)
SI_UNIT($,.METRE.)
);
#5737=(
NAMED_UNIT(*)
PLANE_ANGLE_UNIT()
SI_UNIT($,.RADIAN.)
);
#5738=(
NAMED_UNIT(*)
SI_UNIT($,.STERADIAN.)
SOLID_ANGLE_UNIT()
);
#5739=SHAPE_DEFINITION_REPRESENTATION(#5761,#5808);
#5740=SHAPE_DEFINITION_REPRESENTATION(#5762,#5809);
#5741=SHAPE_DEFINITION_REPRESENTATION(#5763,#5810);
#5742=SHAPE_DEFINITION_REPRESENTATION(#5764,#5811);
#5743=SHAPE_DEFINITION_REPRESENTATION(#5765,#5812);
#5744=SHAPE_DEFINITION_REPRESENTATION(#5766,#5813);
#5745=SHAPE_DEFINITION_REPRESENTATION(#5767,#5814);
#5746=SHAPE_DEFINITION_REPRESENTATION(#5768,#5815);
#5747=SHAPE_DEFINITION_REPRESENTATION(#5769,#5816);
#5748=SHAPE_DEFINITION_REPRESENTATION(#5770,#5817);
#5749=SHAPE_DEFINITION_REPRESENTATION(#5781,#5818);
#5750=SHAPE_DEFINITION_REPRESENTATION(#5782,#5819);
#5751=SHAPE_DEFINITION_REPRESENTATION(#5783,#5820);
#5752=SHAPE_DEFINITION_REPRESENTATION(#5784,#5821);
#5753=SHAPE_DEFINITION_REPRESENTATION(#5785,#5822);
#5754=SHAPE_DEFINITION_REPRESENTATION(#5786,#5823);
#5755=SHAPE_DEFINITION_REPRESENTATION(#5787,#5824);
#5756=SHAPE_DEFINITION_REPRESENTATION(#5788,#5825);
#5757=SHAPE_DEFINITION_REPRESENTATION(#5794,#5826);
#5758=SHAPE_DEFINITION_REPRESENTATION(#5800,#5827);
#5759=SHAPE_DEFINITION_REPRESENTATION(#5801,#5828);
#5760=SHAPE_DEFINITION_REPRESENTATION(#5802,#5829);
#5761=PRODUCT_DEFINITION_SHAPE('',$,#5831);
#5762=PRODUCT_DEFINITION_SHAPE('',$,#5832);
#5763=PRODUCT_DEFINITION_SHAPE('',$,#5833);
#5764=PRODUCT_DEFINITION_SHAPE('',$,#5834);
#5765=PRODUCT_DEFINITION_SHAPE('',$,#5835);
#5766=PRODUCT_DEFINITION_SHAPE('',$,#5836);
#5767=PRODUCT_DEFINITION_SHAPE('',$,#5837);
#5768=PRODUCT_DEFINITION_SHAPE('',$,#5838);
#5769=PRODUCT_DEFINITION_SHAPE('',$,#5839);
#5770=PRODUCT_DEFINITION_SHAPE('',$,#5840);
#5771=PRODUCT_DEFINITION_SHAPE($,$,#116);
#5772=PRODUCT_DEFINITION_SHAPE($,$,#117);
#5773=PRODUCT_DEFINITION_SHAPE($,$,#118);
#5774=PRODUCT_DEFINITION_SHAPE($,$,#119);
#5775=PRODUCT_DEFINITION_SHAPE($,$,#120);
#5776=PRODUCT_DEFINITION_SHAPE($,$,#121);
#5777=PRODUCT_DEFINITION_SHAPE($,$,#122);
#5778=PRODUCT_DEFINITION_SHAPE($,$,#123);
#5779=PRODUCT_DEFINITION_SHAPE($,$,#124);
#5780=PRODUCT_DEFINITION_SHAPE($,$,#125);
#5781=PRODUCT_DEFINITION_SHAPE('',$,#5841);
#5782=PRODUCT_DEFINITION_SHAPE('',$,#5842);
#5783=PRODUCT_DEFINITION_SHAPE('',$,#5843);
#5784=PRODUCT_DEFINITION_SHAPE('',$,#5844);
#5785=PRODUCT_DEFINITION_SHAPE('',$,#5845);
#5786=PRODUCT_DEFINITION_SHAPE('',$,#5846);
#5787=PRODUCT_DEFINITION_SHAPE('',$,#5847);
#5788=PRODUCT_DEFINITION_SHAPE('',$,#5848);
#5789=PRODUCT_DEFINITION_SHAPE($,$,#126);
#5790=PRODUCT_DEFINITION_SHAPE($,$,#127);
#5791=PRODUCT_DEFINITION_SHAPE($,$,#128);
#5792=PRODUCT_DEFINITION_SHAPE($,$,#129);
#5793=PRODUCT_DEFINITION_SHAPE($,$,#130);
#5794=PRODUCT_DEFINITION_SHAPE('',$,#5849);
#5795=PRODUCT_DEFINITION_SHAPE($,$,#131);
#5796=PRODUCT_DEFINITION_SHAPE($,$,#132);
#5797=PRODUCT_DEFINITION_SHAPE($,$,#133);
#5798=PRODUCT_DEFINITION_SHAPE($,$,#134);
#5799=PRODUCT_DEFINITION_SHAPE($,$,#135);
#5800=PRODUCT_DEFINITION_SHAPE('',$,#5850);
#5801=PRODUCT_DEFINITION_SHAPE('',$,#5851);
#5802=PRODUCT_DEFINITION_SHAPE('',$,#5852);
#5803=PRODUCT_DEFINITION_SHAPE($,$,#136);
#5804=PRODUCT_DEFINITION_SHAPE($,$,#137);
#5805=PRODUCT_DEFINITION_SHAPE($,$,#138);
#5806=PRODUCT_DEFINITION_SHAPE($,$,#139);
#5807=PRODUCT_DEFINITION_SHAPE($,$,#140);
#5808=SHAPE_REPRESENTATION('',(#3200,#3558,#3559,#3560),#5712);
#5809=SHAPE_REPRESENTATION('',(#3201,#3359,#3360,#3361,#3362,#3363,#3364,
#3365,#3366,#3367,#3368),#5713);
#5810=SHAPE_REPRESENTATION('',(#3202),#5714);
#5811=SHAPE_REPRESENTATION('',(#3261),#5715);
#5812=SHAPE_REPRESENTATION('',(#3275),#5716);
#5813=SHAPE_REPRESENTATION('',(#3284),#5717);
#5814=SHAPE_REPRESENTATION('',(#3293),#5718);
#5815=SHAPE_REPRESENTATION('',(#3317),#5719);
#5816=SHAPE_REPRESENTATION('',(#3326),#5720);
#5817=SHAPE_REPRESENTATION('',(#3343),#5721);
#5818=SHAPE_REPRESENTATION('',(#3369,#3524,#3525,#3526,#3527,#3528),#5722);
#5819=SHAPE_REPRESENTATION('',(#3370),#5723);
#5820=SHAPE_REPRESENTATION('',(#3387,#3510,#3511,#3512,#3513,#3514),#5724);
#5821=SHAPE_REPRESENTATION('',(#3388),#5725);
#5822=SHAPE_REPRESENTATION('',(#3408),#5726);
#5823=SHAPE_REPRESENTATION('',(#3428),#5727);
#5824=SHAPE_REPRESENTATION('',(#3443),#5728);
#5825=SHAPE_REPRESENTATION('',(#3493),#5729);
#5826=SHAPE_REPRESENTATION('',(#3515),#5730);
#5827=SHAPE_REPRESENTATION('',(#3529,#3556,#3557),#5731);
#5828=SHAPE_REPRESENTATION('',(#3530),#5732);
#5829=SHAPE_REPRESENTATION('',(#3549),#5733);
#5830=PRODUCT_DEFINITION_CONTEXT('part definition',#5898,'design');
#5831=PRODUCT_DEFINITION('PAT-078','PAT-078',#5853,#5830);
#5832=PRODUCT_DEFINITION('Mounting fork and axle',
'Mounting fork and axle',#5854,#5830);
#5833=PRODUCT_DEFINITION('Fixed fork with pedal bearings',
'Fixed fork with pedal bearings',#5855,#5830);
#5834=PRODUCT_DEFINITION('Twelve millimetre dead axle',
'Twelve millimetre dead axle',#5856,#5830);
#5835=PRODUCT_DEFINITION('Inner race spacer','Inner race spacer',#5857,
#5830);
#5836=PRODUCT_DEFINITION('Axle keeper','Axle keeper',#5858,#5830);
#5837=PRODUCT_DEFINITION('M4x10 Cap Screw','M4x10 Cap Screw',#5859,#5830);
#5838=PRODUCT_DEFINITION('Flat Washer - M6','Flat Washer - M6',#5860,#5830);
#5839=PRODUCT_DEFINITION('Hex Bolt - M6 x 30 mm',
'Hex Bolt - M6 x 30 mm',#5861,#5830);
#5840=PRODUCT_DEFINITION('Hex Nut - M6','Hex Nut - M6',#5862,#5830);
#5841=PRODUCT_DEFINITION('Wheel and bearings','Wheel and bearings',#5863,
#5830);
#5842=PRODUCT_DEFINITION('Wheel with twelve millimetre bearings',
'Wheel with twelve millimetre bearings',#5864,#5830);
#5843=PRODUCT_DEFINITION('Sealed Ball Bearing - 12 x 32 x 10 mm',
'Sealed Ball Bearing - 12 x 32 x 10 mm',#5865,#5830);
#5844=PRODUCT_DEFINITION('Inner ring','Inner ring',#5866,#5830);
#5845=PRODUCT_DEFINITION('Outer ring','Outer ring',#5867,#5830);
#5846=PRODUCT_DEFINITION('Balls','Balls',#5868,#5830);
#5847=PRODUCT_DEFINITION('Cage','Cage',#5869,#5830);
#5848=PRODUCT_DEFINITION('Seals 2RS','Seals 2RS',#5870,#5830);
#5849=PRODUCT_DEFINITION('Bearing end retainer','Bearing end retainer',
#5871,#5830);
#5850=PRODUCT_DEFINITION('Friction-set brake pedal',
'Friction-set brake pedal',#5872,#5830);
#5851=PRODUCT_DEFINITION('Brake pedal','Brake pedal',#5873,#5830);
#5852=PRODUCT_DEFINITION('Tread brake pad','Tread brake pad',#5874,#5830);
#5853=PRODUCT_DEFINITION_FORMATION('',$,#5900);
#5854=PRODUCT_DEFINITION_FORMATION('',$,#5901);
#5855=PRODUCT_DEFINITION_FORMATION('',$,#5902);
#5856=PRODUCT_DEFINITION_FORMATION('',$,#5903);
#5857=PRODUCT_DEFINITION_FORMATION('',$,#5904);
#5858=PRODUCT_DEFINITION_FORMATION('',$,#5905);
#5859=PRODUCT_DEFINITION_FORMATION('',$,#5906);
#5860=PRODUCT_DEFINITION_FORMATION('',$,#5907);
#5861=PRODUCT_DEFINITION_FORMATION('',$,#5908);
#5862=PRODUCT_DEFINITION_FORMATION('',$,#5909);
#5863=PRODUCT_DEFINITION_FORMATION('',$,#5910);
#5864=PRODUCT_DEFINITION_FORMATION('',$,#5911);
#5865=PRODUCT_DEFINITION_FORMATION('',$,#5912);
#5866=PRODUCT_DEFINITION_FORMATION('',$,#5913);
#5867=PRODUCT_DEFINITION_FORMATION('',$,#5914);
#5868=PRODUCT_DEFINITION_FORMATION('',$,#5915);
#5869=PRODUCT_DEFINITION_FORMATION('',$,#5916);
#5870=PRODUCT_DEFINITION_FORMATION('',$,#5917);
#5871=PRODUCT_DEFINITION_FORMATION('',$,#5918);
#5872=PRODUCT_DEFINITION_FORMATION('',$,#5919);
#5873=PRODUCT_DEFINITION_FORMATION('',$,#5920);
#5874=PRODUCT_DEFINITION_FORMATION('',$,#5921);
#5875=PRODUCT_RELATED_PRODUCT_CATEGORY('PAT-078','PAT-078',(#5900));
#5876=PRODUCT_RELATED_PRODUCT_CATEGORY('Mounting fork and axle',
'Mounting fork and axle',(#5901));
#5877=PRODUCT_RELATED_PRODUCT_CATEGORY('Fixed fork with pedal bearings',
'Fixed fork with pedal bearings',(#5902));
#5878=PRODUCT_RELATED_PRODUCT_CATEGORY('Twelve millimetre dead axle',
'Twelve millimetre dead axle',(#5903));
#5879=PRODUCT_RELATED_PRODUCT_CATEGORY('Inner race spacer',
'Inner race spacer',(#5904));
#5880=PRODUCT_RELATED_PRODUCT_CATEGORY('Axle keeper','Axle keeper',(#5905));
#5881=PRODUCT_RELATED_PRODUCT_CATEGORY('M4x10 Cap Screw',
'M4x10 Cap Screw',(#5906));
#5882=PRODUCT_RELATED_PRODUCT_CATEGORY('Flat Washer - M6',
'Flat Washer - M6',(#5907));
#5883=PRODUCT_RELATED_PRODUCT_CATEGORY('Hex Bolt - M6 x 30 mm',
'Hex Bolt - M6 x 30 mm',(#5908));
#5884=PRODUCT_RELATED_PRODUCT_CATEGORY('Hex Nut - M6','Hex Nut - M6',(#5909));
#5885=PRODUCT_RELATED_PRODUCT_CATEGORY('Wheel and bearings',
'Wheel and bearings',(#5910));
#5886=PRODUCT_RELATED_PRODUCT_CATEGORY(
'Wheel with twelve millimetre bearings',
'Wheel with twelve millimetre bearings',(#5911));
#5887=PRODUCT_RELATED_PRODUCT_CATEGORY(
'Sealed Ball Bearing - 12 x 32 x 10 mm',
'Sealed Ball Bearing - 12 x 32 x 10 mm',(#5912));
#5888=PRODUCT_RELATED_PRODUCT_CATEGORY('Inner ring','Inner ring',(#5913));
#5889=PRODUCT_RELATED_PRODUCT_CATEGORY('Outer ring','Outer ring',(#5914));
#5890=PRODUCT_RELATED_PRODUCT_CATEGORY('Balls','Balls',(#5915));
#5891=PRODUCT_RELATED_PRODUCT_CATEGORY('Cage','Cage',(#5916));
#5892=PRODUCT_RELATED_PRODUCT_CATEGORY('Seals 2RS','Seals 2RS',(#5917));
#5893=PRODUCT_RELATED_PRODUCT_CATEGORY('Bearing end retainer',
'Bearing end retainer',(#5918));
#5894=PRODUCT_RELATED_PRODUCT_CATEGORY('Friction-set brake pedal',
'Friction-set brake pedal',(#5919));
#5895=PRODUCT_RELATED_PRODUCT_CATEGORY('Brake pedal','Brake pedal',(#5920));
#5896=PRODUCT_RELATED_PRODUCT_CATEGORY('Tread brake pad',
'Tread brake pad',(#5921));
#5897=APPLICATION_PROTOCOL_DEFINITION('international standard',
'automotive_design',2009,#5898);
#5898=APPLICATION_CONTEXT(
'Core Data for Automotive Mechanical Design Process');
#5899=PRODUCT_CONTEXT('part definition',#5898,'mechanical');
#5900=PRODUCT('PAT-078','PAT-078',
'PAT-078',(#5899));
#5901=PRODUCT('Mounting fork and axle','Mounting fork and axle',
'Mounting fork and axle',(#5899));
#5902=PRODUCT('Fixed fork with pedal bearings',
'Fixed fork with pedal bearings','Fixed fork with pedal bearings',(#5899));
#5903=PRODUCT('Twelve millimetre dead axle',
'Twelve millimetre dead axle','Twelve millimetre dead axle',(#5899));
#5904=PRODUCT('Inner race spacer','Inner race spacer',
'Inner race spacer',(#5899));
#5905=PRODUCT('Axle keeper','Axle keeper','Axle keeper',(#5899));
#5906=PRODUCT('M4x10 Cap Screw','M4x10 Cap Screw','M4x10 Cap Screw',(#5899));
#5907=PRODUCT('Flat Washer - M6','Flat Washer - M6','Flat Washer - M6',
(#5899));
#5908=PRODUCT('Hex Bolt - M6 x 30 mm','Hex Bolt - M6 x 30 mm',
'Hex Bolt - M6 x 30 mm',(#5899));
#5909=PRODUCT('Hex Nut - M6','Hex Nut - M6','Hex Nut - M6',(#5899));
#5910=PRODUCT('Wheel and bearings','Wheel and bearings',
'Wheel and bearings',(#5899));
#5911=PRODUCT('Wheel with twelve millimetre bearings',
'Wheel with twelve millimetre bearings',
'Wheel with twelve millimetre bearings',(#5899));
#5912=PRODUCT('Sealed Ball Bearing - 12 x 32 x 10 mm',
'Sealed Ball Bearing - 12 x 32 x 10 mm',
'Sealed Ball Bearing - 12 x 32 x 10 mm',(#5899));
#5913=PRODUCT('Inner ring','Inner ring','Inner ring',(#5899));
#5914=PRODUCT('Outer ring','Outer ring','Outer ring',(#5899));
#5915=PRODUCT('Balls','Balls','Balls',(#5899));
#5916=PRODUCT('Cage','Cage','Cage',(#5899));
#5917=PRODUCT('Seals 2RS','Seals 2RS','Seals 2RS',(#5899));
#5918=PRODUCT('Bearing end retainer','Bearing end retainer',
'Bearing end retainer',(#5899));
#5919=PRODUCT('Friction-set brake pedal','Friction-set brake pedal',
'Friction-set brake pedal',(#5899));
#5920=PRODUCT('Brake pedal','Brake pedal','Brake pedal',(#5899));
#5921=PRODUCT('Tread brake pad','Tread brake pad','Tread brake pad',(#5899));
#5922=PRESENTATION_STYLE_ASSIGNMENT((#5927));
#5923=PRESENTATION_STYLE_ASSIGNMENT((#5928));
#5924=PRESENTATION_STYLE_ASSIGNMENT((#5929));
#5925=PRESENTATION_STYLE_ASSIGNMENT((#5930));
#5926=PRESENTATION_STYLE_ASSIGNMENT((#5931));
#5927=SURFACE_STYLE_USAGE(.BOTH.,#5932);
#5928=SURFACE_STYLE_USAGE(.BOTH.,#5933);
#5929=SURFACE_STYLE_USAGE(.BOTH.,#5934);
#5930=SURFACE_STYLE_USAGE(.BOTH.,#5935);
#5931=SURFACE_STYLE_USAGE(.BOTH.,#5936);
#5932=SURFACE_SIDE_STYLE('',(#5937));
#5933=SURFACE_SIDE_STYLE('',(#5938));
#5934=SURFACE_SIDE_STYLE('',(#5939));
#5935=SURFACE_SIDE_STYLE('',(#5940));
#5936=SURFACE_SIDE_STYLE('',(#5941));
#5937=SURFACE_STYLE_FILL_AREA(#5942);
#5938=SURFACE_STYLE_FILL_AREA(#5943);
#5939=SURFACE_STYLE_FILL_AREA(#5944);
#5940=SURFACE_STYLE_FILL_AREA(#5945);
#5941=SURFACE_STYLE_FILL_AREA(#5946);
#5942=FILL_AREA_STYLE('Steel - Satin',(#5947));
#5943=FILL_AREA_STYLE('CAD Library Painted - Steel gray',(#5948));
#5944=FILL_AREA_STYLE('CAD Library Painted - Engineering blue',(#5949));
#5945=FILL_AREA_STYLE('CAD Library Painted - Graphite',(#5950));
#5946=FILL_AREA_STYLE('CAD Library Painted - Off white',(#5951));
#5947=FILL_AREA_STYLE_COLOUR('Steel - Satin',#5952);
#5948=FILL_AREA_STYLE_COLOUR('CAD Library Painted - Steel gray',#5953);
#5949=FILL_AREA_STYLE_COLOUR('CAD Library Painted - Engineering blue',#5954);
#5950=FILL_AREA_STYLE_COLOUR('CAD Library Painted - Graphite',#5955);
#5951=FILL_AREA_STYLE_COLOUR('CAD Library Painted - Off white',#5956);
#5952=COLOUR_RGB('Steel - Satin',0.627450980392157,0.627450980392157,0.627450980392157);
#5953=COLOUR_RGB('CAD Library Painted - Steel gray',0.592156862745098,0.631372549019608,
0.67843137254902);
#5954=COLOUR_RGB('CAD Library Painted - Engineering blue',0.12156862745098,
0.356862745098039,0.6);
#5955=COLOUR_RGB('CAD Library Painted - Graphite',0.0980392156862745,0.109803921568627,
0.125490196078431);
#5956=COLOUR_RGB('CAD Library Painted - Off white',0.909803921568627,0.901960784313726,
0.858823529411765);
#5957=COLOUR_RGB('Dark Blue',0.08,0.2,0.34);
#5958=FILL_AREA_STYLE_COLOUR('',#5957);
#5959=FILL_AREA_STYLE('',(#5958));
#5960=SURFACE_STYLE_FILL_AREA(#5959);
#5961=SURFACE_SIDE_STYLE('',(#5960));
#5962=SURFACE_STYLE_USAGE(.BOTH.,#5961);
#5963=PRESENTATION_STYLE_ASSIGNMENT((#5962));
#5964=COLOUR_RGB('Light Blue',0.38,0.62,0.78);
#5965=FILL_AREA_STYLE_COLOUR('',#5964);
#5966=FILL_AREA_STYLE('',(#5965));
#5967=SURFACE_STYLE_FILL_AREA(#5966);
#5968=SURFACE_SIDE_STYLE('',(#5967));
#5969=SURFACE_STYLE_USAGE(.BOTH.,#5968);
#5970=PRESENTATION_STYLE_ASSIGNMENT((#5969));
#5971=COLOUR_RGB('Sky Blue',0.24,0.69,0.87);
#5972=FILL_AREA_STYLE_COLOUR('',#5971);
#5973=FILL_AREA_STYLE('',(#5972));
#5974=SURFACE_STYLE_FILL_AREA(#5973);
#5975=SURFACE_SIDE_STYLE('',(#5974));
#5976=SURFACE_STYLE_USAGE(.BOTH.,#5975);
#5977=PRESENTATION_STYLE_ASSIGNMENT((#5976));
#5978=COLOUR_RGB('Grey',0.48,0.52,0.57);
#5979=FILL_AREA_STYLE_COLOUR('',#5978);
#5980=FILL_AREA_STYLE('',(#5979));
#5981=SURFACE_STYLE_FILL_AREA(#5980);
#5982=SURFACE_SIDE_STYLE('',(#5981));
#5983=SURFACE_STYLE_USAGE(.BOTH.,#5982);
#5984=PRESENTATION_STYLE_ASSIGNMENT((#5983));
#5985=COLOUR_RGB('Black',0.12,0.14,0.17);
#5986=FILL_AREA_STYLE_COLOUR('',#5985);
#5987=FILL_AREA_STYLE('',(#5986));
#5988=SURFACE_STYLE_FILL_AREA(#5987);
#5989=SURFACE_SIDE_STYLE('',(#5988));
#5990=SURFACE_STYLE_USAGE(.BOTH.,#5989);
#5991=PRESENTATION_STYLE_ASSIGNMENT((#5990));
#5992=COLOUR_RGB('Off White',0.89,0.88,0.83);
#5993=FILL_AREA_STYLE_COLOUR('',#5992);
#5994=FILL_AREA_STYLE('',(#5993));
#5995=SURFACE_STYLE_FILL_AREA(#5994);
#5996=SURFACE_SIDE_STYLE('',(#5995));
#5997=SURFACE_STYLE_USAGE(.BOTH.,#5996);
#5998=PRESENTATION_STYLE_ASSIGNMENT((#5997));
ENDSEC;
END-ISO-10303-21;
